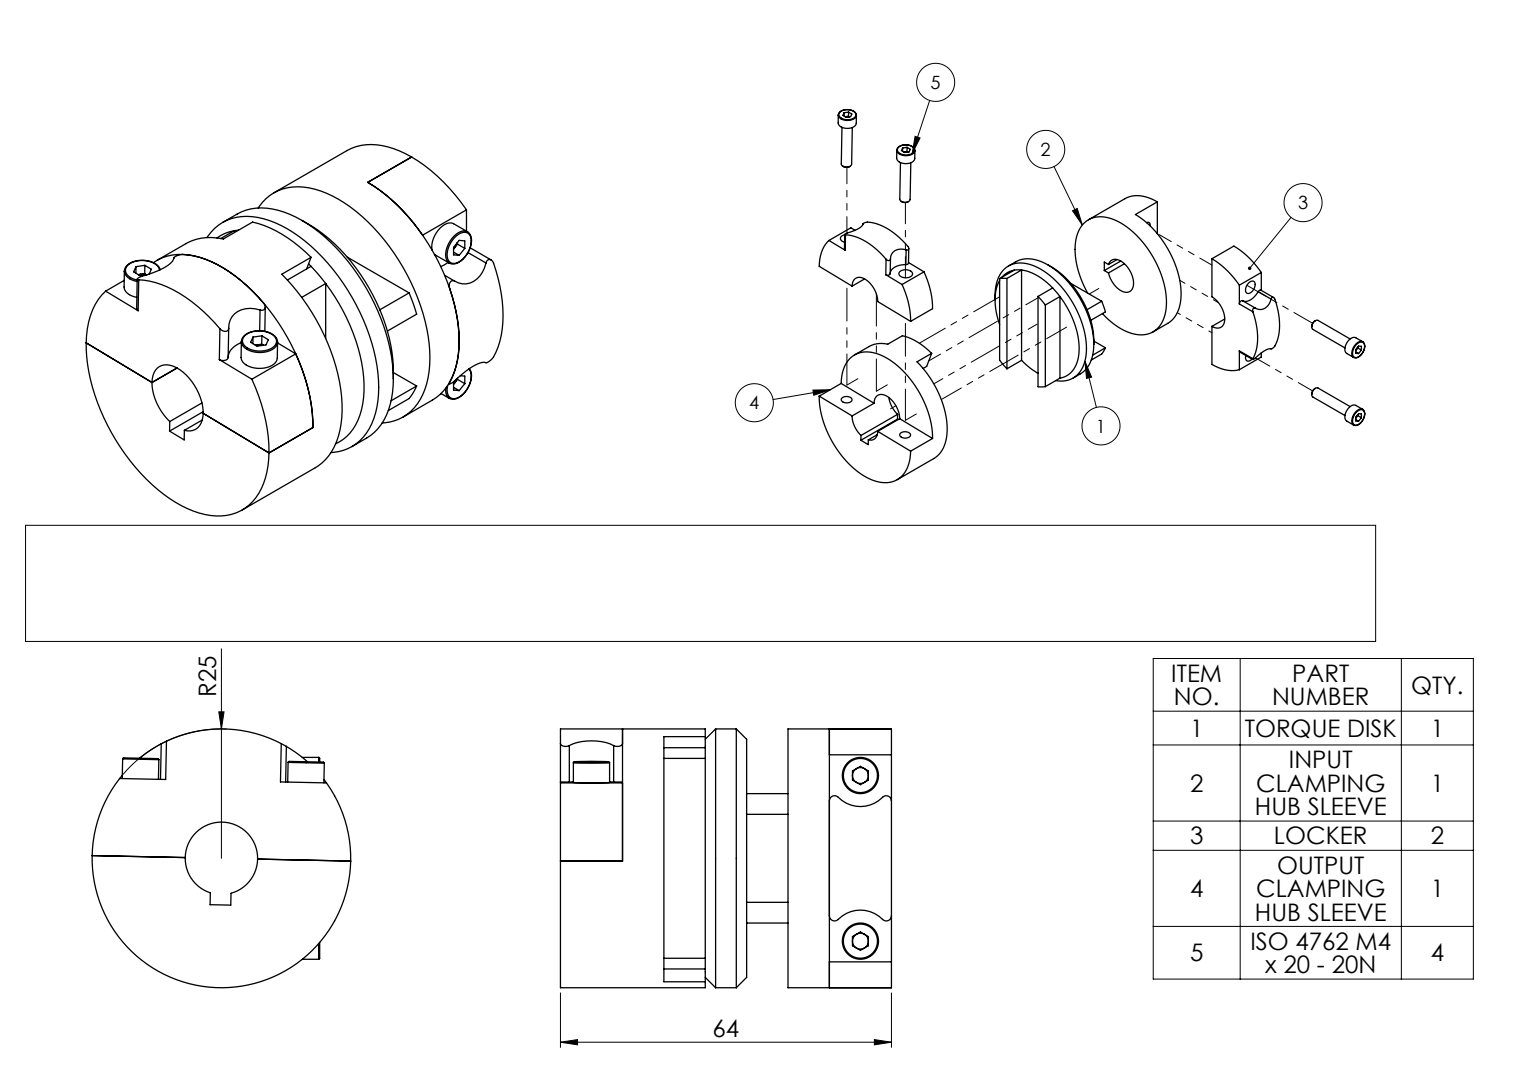
ISO-10303-21;
HEADER;
FILE_DESCRIPTION (('STEP AP214'),
    '1' );
FILE_NAME ('BR-550',
    '2026-10-08T14:09:18',
    ( '' ),
    ( '' ),
    'SwSTEP 2.0',
    'SolidWorks 2026',
    '' );
FILE_SCHEMA (( 'AUTOMOTIVE_DESIGN' ));
ENDSEC;

DATA;
#1 = LINE ( 'NONE', #1937, #4329 ) ;
#2 = CARTESIAN_POINT ( 'NONE',  ( -6.517431832507181422E-14, 16.00000000000000000, -26.00000000000000355 ) ) ;
#3 = EDGE_LOOP ( 'NONE', ( #3250, #4536, #2732 ) ) ;
#4 = CARTESIAN_POINT ( 'NONE',  ( 0.000000000000000000, 0.000000000000000000, -12.00000000000000000 ) ) ;
#5 = AXIS2_PLACEMENT_3D ( 'NONE', #3716, #3077, #4925 ) ;
#6 = AXIS2_PLACEMENT_3D ( 'NONE', #3174, #4687, #3807 ) ;
#7 = VERTEX_POINT ( 'NONE', #1885 ) ;
#8 = EDGE_CURVE ( 'NONE', #881, #1919, #4427, .T. ) ;
#9 = VERTEX_POINT ( 'NONE', #2215 ) ;
#10 =( NAMED_UNIT ( * ) PLANE_ANGLE_UNIT ( ) SI_UNIT ( $, .RADIAN. ) );
#11 = EDGE_CURVE ( 'NONE', #1059, #406, #4156, .T. ) ;
#12 = VECTOR ( 'NONE', #1631, 1000.000000000000227 ) ;
#13 = DIRECTION ( 'NONE',  ( -0.000000000000000000, -0.000000000000000000, 1.000000000000000000 ) ) ;
#14 = CIRCLE ( 'NONE', #4735, 1.535500000000000087 ) ;
#15 = CARTESIAN_POINT ( 'NONE',  ( -6.708203932499367639, 2.000000000000000888, -20.00000000000000000 ) ) ;
#16 = ORIENTED_EDGE ( 'NONE', *, *, #4419, .T. ) ;
#17 = AXIS2_PLACEMENT_3D ( 'NONE', #2780, #4294, #3843 ) ;
#18 = ADVANCED_FACE ( 'NONE', ( #4455 ), #1426, .T. ) ;
#19 = ADVANCED_FACE ( 'NONE', ( #264 ), #4482, .F. ) ;
#20 = CARTESIAN_POINT ( 'NONE',  ( 2.500000000000000000, -1.178949249685218303, -2.041999999999998039 ) ) ;
#21 = AXIS2_PLACEMENT_3D ( 'NONE', #885, #4593, #1214 ) ;
#22 = EDGE_LOOP ( 'NONE', ( #4472, #3909, #3003, #3741, #4316 ) ) ;
#23 = ORIENTED_EDGE ( 'NONE', *, *, #1515, .T. ) ;
#24 = CIRCLE ( 'NONE', #1949, 3.500000000000000000 ) ;
#25 = CARTESIAN_POINT ( 'NONE',  ( 22.89074894326665088, 10.05057747304974924, -26.80355754512474675 ) ) ;
#26 = FACE_OUTER_BOUND ( 'NONE', #3587, .T. ) ;
#27 = DIRECTION ( 'NONE',  ( 0.000000000000000000, -1.000000000000000000, 1.287488025362403787E-15 ) ) ;
#28 = CIRCLE ( 'NONE', #4350, 3.500000000000000000 ) ;
#29 = DIRECTION ( 'NONE',  ( -0.000000000000000000, -0.000000000000000000, 1.000000000000000000 ) ) ;
#30 = ORIENTED_EDGE ( 'NONE', *, *, #808, .T. ) ;
#31 = DIRECTION ( 'NONE',  ( 1.000000000000000000, 0.000000000000000000, 0.000000000000000000 ) ) ;
#32 = CARTESIAN_POINT ( 'NONE',  ( 15.00000000000000178, -16.00000000000000000, -26.00000000000000355 ) ) ;
#33 = DIRECTION ( 'NONE',  ( -0.000000000000000000, 1.000000000000000000, 1.224646799147353207E-16 ) ) ;
#34 = FACE_BOUND ( 'NONE', #887, .T. ) ;
#35 = CIRCLE ( 'NONE', #4595, 22.99999999999998934 ) ;
#36 = ORIENTED_EDGE ( 'NONE', *, *, #664, .F. ) ;
#37 = EDGE_LOOP ( 'NONE', ( #3778, #2575, #3763, #206 ) ) ;
#38 = ADVANCED_BREP_SHAPE_REPRESENTATION ( '', ( #2058, #1918 ), #1039 ) ;
#39 = DIRECTION ( 'NONE',  ( 0.000000000000000000, 0.000000000000000000, -1.000000000000000000 ) ) ;
#40 = FACE_OUTER_BOUND ( 'NONE', #1799, .T. ) ;
#41 = LINE ( 'NONE', #2781, #4907 ) ;
#42 = ORIENTED_EDGE ( 'NONE', *, *, #4705, .F. ) ;
#43 = DIRECTION ( 'NONE',  ( 1.000000000000000000, -0.000000000000000000, -0.000000000000000000 ) ) ;
#44 = LINE ( 'NONE', #3926, #164 ) ;
#45 = VERTEX_POINT ( 'NONE', #656 ) ;
#46 = PRODUCT_DEFINITION_SHAPE ( 'NONE', 'NONE',  #4967 ) ;
#47 = ADVANCED_FACE ( 'NONE', ( #2594 ), #1860, .F. ) ;
#48 = EDGE_LOOP ( 'NONE', ( #130, #2080, #1685, #2442 ) ) ;
#49 = LINE ( 'NONE', #3799, #2903 ) ;
#50 = FACE_OUTER_BOUND ( 'NONE', #3870, .T. ) ;
#51 = PRODUCT ( 'socket head cap screw_iso_ISO 4762 M5 x 20 - 20N', 'socket head cap screw_iso_ISO 4762 M5 x 20 - 20N', '', ( #972 ) ) ;
#52 = DIRECTION ( 'NONE',  ( -1.000000000000000000, -0.000000000000000000, -0.000000000000000000 ) ) ;
#53 = EDGE_CURVE ( 'NONE', #754, #3692, #3957, .T. ) ;
#54 = VERTEX_POINT ( 'NONE', #3686 ) ;
#55 = ORIENTED_EDGE ( 'NONE', *, *, #2270, .T. ) ;
#56 = DIRECTION ( 'NONE',  ( 0.000000000000000000, 0.000000000000000000, -1.000000000000000000 ) ) ;
#57 = DIRECTION ( 'NONE',  ( 1.000000000000000000, 0.000000000000000000, 0.000000000000000000 ) ) ;
#58 = FACE_OUTER_BOUND ( 'NONE', #389, .T. ) ;
#59 = ORIENTED_EDGE ( 'NONE', *, *, #2870, .T. ) ;
#60 = ORIENTED_EDGE ( 'NONE', *, *, #3152, .T. ) ;
#61 =( NAMED_UNIT ( * ) PLANE_ANGLE_UNIT ( ) SI_UNIT ( $, .RADIAN. ) );
#62 = CARTESIAN_POINT ( 'NONE',  ( 0.000000000000000000, 0.000000000000000000, 4.000000000000000000 ) ) ;
#63 = DIRECTION ( 'NONE',  ( 1.000000000000000000, -0.000000000000000000, 0.000000000000000000 ) ) ;
#64 = DIRECTION ( 'NONE',  ( 0.000000000000000000, -1.000000000000000000, 0.000000000000000000 ) ) ;
#65 = PRESENTATION_LAYER_ASSIGNMENT (  '', '', ( #1267 ) ) ;
#66 = ORIENTED_EDGE ( 'NONE', *, *, #2378, .T. ) ;
#67 = CARTESIAN_POINT ( 'NONE',  ( 25.00000000000000000, -11.80087472665741011, -21.71428571428571530 ) ) ;
#68 = EDGE_LOOP ( 'NONE', ( #4400, #3556, #1967, #1620 ) ) ;
#69 = ORIENTED_EDGE ( 'NONE', *, *, #2839, .T. ) ;
#70 = ADVANCED_FACE ( 'NONE', ( #1108 ), #102, .F. ) ;
#71 = ADVANCED_FACE ( 'NONE', ( #4306 ), #1906, .T. ) ;
#72 = CARTESIAN_POINT ( 'NONE',  ( 22.90859662698202470, -10.00982993400317334, -25.60100662543646877 ) ) ;
#73 = DIRECTION ( 'NONE',  ( 1.000000000000000000, -0.000000000000000000, -0.000000000000000000 ) ) ;
#74 = CARTESIAN_POINT ( 'NONE',  ( 2.000000000000000000, 1.329782007511006281, 0.7677499999999990443 ) ) ;
#75 = ORIENTED_EDGE ( 'NONE', *, *, #4606, .T. ) ;
#76 = AXIS2_PLACEMENT_3D ( 'NONE', #1953, #1896, #4546 ) ;
#77 = EDGE_LOOP ( 'NONE', ( #2842, #2826, #4730, #3841 ) ) ;
#78 = EDGE_CURVE ( 'NONE', #3692, #754, #3167, .T. ) ;
#79 = DIRECTION ( 'NONE',  ( 1.000000000000000000, 0.000000000000000000, 0.000000000000000000 ) ) ;
#80 = DIRECTION ( 'NONE',  ( -0.000000000000000000, -0.000000000000000000, 1.000000000000000000 ) ) ;
#81 = CARTESIAN_POINT ( 'NONE',  ( 21.90226041726126383, 12.05376714070078847, -31.32044994803182547 ) ) ;
#82 = ORIENTED_EDGE ( 'NONE', *, *, #1120, .T. ) ;
#83 = AXIS2_PLACEMENT_3D ( 'NONE', #3595, #2177, #3698 ) ;
#84 = ORIENTED_EDGE ( 'NONE', *, *, #4675, .T. ) ;
#85 = SURFACE_STYLE_FILL_AREA ( #4292 ) ;
#86 = DIRECTION ( 'NONE',  ( 1.000000000000000000, 0.000000000000000000, -0.000000000000000000 ) ) ;
#87 = DIRECTION ( 'NONE',  ( 1.357798298438996130E-15, -1.000000000000000000, 0.000000000000000000 ) ) ;
#88 = CARTESIAN_POINT ( 'NONE',  ( 15.00000000000000000, 11.10102051443364424, -21.00000000000000000 ) ) ;
#89 = AXIS2_PLACEMENT_3D ( 'NONE', #3740, #316, #1588 ) ;
#90 = ORIENTED_EDGE ( 'NONE', *, *, #4505, .T. ) ;
#91 = CIRCLE ( 'NONE', #3370, 2.099999999999997868 ) ;
#92 = VECTOR ( 'NONE', #1190, 1000.000000000000000 ) ;
#93 = LINE ( 'NONE', #2056, #2959 ) ;
#94 = DIRECTION ( 'NONE',  ( -1.000000000000000000, 0.000000000000000000, 0.000000000000000000 ) ) ;
#95 = ORIENTED_EDGE ( 'NONE', *, *, #1051, .F. ) ;
#96 = VECTOR ( 'NONE', #306, 1000.000000000000000 ) ;
#97 = VECTOR ( 'NONE', #3015, 1000.000000000000000 ) ;
#98 = ORIENTED_EDGE ( 'NONE', *, *, #3653, .F. ) ;
#99 = EDGE_CURVE ( 'NONE', #4080, #934, #4271, .T. ) ;
#100 = CIRCLE ( 'NONE', #2908, 6.999999999999999112 ) ;
#101 = AXIS2_PLACEMENT_3D ( 'NONE', #4841, #1750, #2213 ) ;
#102 = PLANE ( 'NONE',  #3242 ) ;
#103 = VECTOR ( 'NONE', #177, 1000.000000000000114 ) ;
#104 = CARTESIAN_POINT ( 'NONE',  ( 22.03949535914419755, -11.80087472665740655, -21.71428571428571885 ) ) ;
#105 = FACE_OUTER_BOUND ( 'NONE', #4278, .T. ) ;
#106 = CARTESIAN_POINT ( 'NONE',  ( 2.000000000000000000, -1.773042676681340968, 2.059984127722458425E-15 ) ) ;
#107 = VERTEX_POINT ( 'NONE', #3557 ) ;
#108 = SHAPE_DEFINITION_REPRESENTATION ( #4246, #4748 ) ;
#109 = CIRCLE ( 'NONE', #436, 17.00000000000000000 ) ;
#110 = DIRECTION ( 'NONE',  ( 0.000000000000000000, -0.4999999999999993339, 0.8660254037844389297 ) ) ;
#111 = CARTESIAN_POINT ( 'NONE',  ( -9.000000000000003553, -1.999999999999999112, -20.00000000000000000 ) ) ;
#112 = CARTESIAN_POINT ( 'NONE',  ( 0.000000000000000000, 0.000000000000000000, -20.00000000000000000 ) ) ;
#113 = EDGE_CURVE ( 'NONE', #181, #2456, #4183, .T. ) ;
#114 = ORIENTED_EDGE ( 'NONE', *, *, #457, .T. ) ;
#115 = VERTEX_POINT ( 'NONE', #877 ) ;
#116 = CARTESIAN_POINT ( 'NONE',  ( -25.00000000000000000, 3.061616997868383043E-15, -4.000000000000000000 ) ) ;
#117 = CARTESIAN_POINT ( 'NONE',  ( 0.000000000000000000, 25.00000000000000000, -20.00000000000000000 ) ) ;
#118 = AXIS2_PLACEMENT_3D ( 'NONE', #3711, #1384, #2920 ) ;
#119 = DIRECTION ( 'NONE',  ( 1.000000000000000000, 0.000000000000000000, 0.000000000000000000 ) ) ;
#120 = ADVANCED_FACE ( 'NONE', ( #2037 ), #2439, .T. ) ;
#121 = VERTEX_POINT ( 'NONE', #126 ) ;
#122 = CIRCLE ( 'NONE', #3524, 2.649999999999995914 ) ;
#123 = DIRECTION ( 'NONE',  ( -0.000000000000000000, -0.000000000000000000, -1.000000000000000000 ) ) ;
#124 = CARTESIAN_POINT ( 'NONE',  ( 16.10609822396473945, -5.439999999999995062, -4.000000000000000000 ) ) ;
#125 = EDGE_LOOP ( 'NONE', ( #685, #558, #2484, #4035, #4209, #3718, #4513, #747 ) ) ;
#126 = CARTESIAN_POINT ( 'NONE',  ( -16.10609822396473945, -5.439999999999995062, -12.00000000000000000 ) ) ;
#127 =( NAMED_UNIT ( * ) SI_UNIT ( $, .STERADIAN. ) SOLID_ANGLE_UNIT ( ) );
#128 = DIRECTION ( 'NONE',  ( 0.000000000000000000, -0.8660254037844390407, -0.4999999999999994449 ) ) ;
#129 = EDGE_LOOP ( 'NONE', ( #232, #1337, #3287, #640, #1099, #3548 ) ) ;
#130 = ORIENTED_EDGE ( 'NONE', *, *, #800, .F. ) ;
#131 = PRODUCT_DEFINITION_SHAPE ( 'NONE', 'NONE',  #4966 ) ;
#132 = DIRECTION ( 'NONE',  ( 1.000000000000000000, 2.168404344971009361E-16, 0.000000000000000000 ) ) ;
#133 = EDGE_CURVE ( 'NONE', #4849, #2456, #528, .T. ) ;
#134 = DIRECTION ( 'NONE',  ( 0.7071067811865487940, 0.000000000000000000, 0.7071067811865463515 ) ) ;
#135 = DIRECTION ( 'NONE',  ( 0.5150380749100544886, 0.000000000000000000, -0.8571673007021121116 ) ) ;
#136 = EDGE_LOOP ( 'NONE', ( #1667, #4376 ) ) ;
#137 = SHAPE_REPRESENTATION ( 'BR-550', ( #3910, #1023, #1106, #3114, #2394, #3506, #4703, #4215, #952, #1905 ), #555 ) ;
#138 = ORIENTED_EDGE ( 'NONE', *, *, #3058, .T. ) ;
#139 = SURFACE_STYLE_USAGE ( .BOTH. , #2050 ) ;
#140 = DIRECTION ( 'NONE',  ( 0.000000000000000000, 0.000000000000000000, -1.000000000000000000 ) ) ;
#141 = CYLINDRICAL_SURFACE ( 'NONE', #2344, 2.649999999999992806 ) ;
#142 = DIRECTION ( 'NONE',  ( -1.000000000000000000, 0.000000000000000000, -0.000000000000000000 ) ) ;
#143 = ORIENTED_EDGE ( 'NONE', *, *, #299, .T. ) ;
#144 = DIRECTION ( 'NONE',  ( 1.000000000000000000, -0.000000000000000000, -0.000000000000000000 ) ) ;
#145 = CARTESIAN_POINT ( 'NONE',  ( 25.00000000000000000, 11.80087472665740478, -30.28571428571428470 ) ) ;
#146 = EDGE_CURVE ( 'NONE', #3852, #4296, #1281, .T. ) ;
#147 = CARTESIAN_POINT ( 'NONE',  ( 0.000000000000000000, 0.000000000000000000, -20.00000000000000000 ) ) ;
#148 = VERTEX_POINT ( 'NONE', #905 ) ;
#149 = CARTESIAN_POINT ( 'NONE',  ( -9.999999999999975131, -16.00000000000000000, -28.10000000000000142 ) ) ;
#150 = DIRECTION ( 'NONE',  ( -1.000000000000000000, -4.073394895316987600E-15, 0.000000000000000000 ) ) ;
#151 = LINE ( 'NONE', #2483, #3855 ) ;
#152 = ORIENTED_EDGE ( 'NONE', *, *, #1724, .T. ) ;
#153 = VERTEX_POINT ( 'NONE', #3959 ) ;
#154 = FACE_OUTER_BOUND ( 'NONE', #602, .T. ) ;
#155 = CARTESIAN_POINT ( 'NONE',  ( 15.00000000000000000, 16.00000000000000000, -26.00000000000000355 ) ) ;
#156 = CARTESIAN_POINT ( 'NONE',  ( 22.03949535914419755, -11.80087472665740655, -21.71428571428571885 ) ) ;
#157 = ORIENTED_EDGE ( 'NONE', *, *, #1693, .F. ) ;
#158 = ADVANCED_FACE ( 'NONE', ( #4205 ), #2001, .F. ) ;
#159 = B_SPLINE_CURVE_WITH_KNOTS ( 'NONE', 3,
 ( #3123, #2291, #1168, #2640, #4187, #3835, #3809, #759, #1888, #81, #4617, #385, #2749, #3439, #2697, #3415 ),
 .UNSPECIFIED., .F., .F.,
 ( 4, 2, 2, 2, 2, 2, 2, 4 ),
 ( 0.000000000000000000, 0.0003092645584586380158, 0.0006185291169172760315, 0.0009277936753759139388, 0.001237058233834552063, 0.001546322792293189970, 0.001855587350751827878, 0.002474116467669114968 ),
 .UNSPECIFIED. ) ;
#160 = ORIENTED_EDGE ( 'NONE', *, *, #457, .F. ) ;
#161 = DIRECTION ( 'NONE',  ( -1.000000000000000000, 0.000000000000000000, -0.000000000000000000 ) ) ;
#162 = CARTESIAN_POINT ( 'NONE',  ( 22.40016391766193138, 11.10102051443364424, -20.00000000000000000 ) ) ;
#163 = CARTESIAN_POINT ( 'NONE',  ( 0.1999999999999987899, 0.000000000000000000, 0.000000000000000000 ) ) ;
#164 = VECTOR ( 'NONE', #508, 1000.000000000000000 ) ;
#165 = VERTEX_POINT ( 'NONE', #2693 ) ;
#166 = EDGE_CURVE ( 'NONE', #107, #941, #3578, .T. ) ;
#167 = CARTESIAN_POINT ( 'NONE',  ( -12.50000000000000178, 19.30673457630782863, 4.000000000000000000 ) ) ;
#168 = CARTESIAN_POINT ( 'NONE',  ( 23.68543856465402442, -8.000000000000003553, 14.30577747056276472 ) ) ;
#169 = AXIS2_PLACEMENT_3D ( 'NONE', #62, #3894, #4293 ) ;
#170 = ORIENTED_EDGE ( 'NONE', *, *, #708, .F. ) ;
#171 = CIRCLE ( 'NONE', #2417, 17.00000000000000000 ) ;
#172 = EDGE_CURVE ( 'NONE', #645, #1989, #1795, .T. ) ;
#173 = VECTOR ( 'NONE', #4086, 1000.000000000000000 ) ;
#174 = EDGE_CURVE ( 'NONE', #4395, #54, #1471, .T. ) ;
#175 = DIRECTION ( 'NONE',  ( 0.9474175425861609545, -0.3199999999999996181, 0.000000000000000000 ) ) ;
#176 = CIRCLE ( 'NONE', #732, 3.500000000000000000 ) ;
#177 = DIRECTION ( 'NONE',  ( -0.9474175425861605104, 0.3200000000000010059, 0.000000000000000000 ) ) ;
#178 =( GEOMETRIC_REPRESENTATION_CONTEXT ( 3 ) GLOBAL_UNCERTAINTY_ASSIGNED_CONTEXT ( ( #350 ) ) GLOBAL_UNIT_ASSIGNED_CONTEXT ( ( #3558, #3977, #127 ) ) REPRESENTATION_CONTEXT ( 'NONE', 'WORKASPACE' ) );
#179 = CARTESIAN_POINT ( 'NONE',  ( 23.00000000000000711, 2.939152317953648289E-15, 4.000000000000000000 ) ) ;
#180 = ORIENTED_EDGE ( 'NONE', *, *, #1366, .T. ) ;
#181 = VERTEX_POINT ( 'NONE', #4357 ) ;
#182 = CIRCLE ( 'NONE', #2505, 2.041999999999999815 ) ;
#183 = VECTOR ( 'NONE', #1498, 999.9999999999998863 ) ;
#184 = AXIS2_PLACEMENT_3D ( 'NONE', #4270, #4673, #3105 ) ;
#185 = CARTESIAN_POINT ( 'NONE',  ( 16.10609822396473945, -5.439999999999995062, 14.30577747056276472 ) ) ;
#186 = DIRECTION ( 'NONE',  ( 1.000000000000000000, -1.106769389831504189E-16, 0.000000000000000000 ) ) ;
#187 = AXIS2_PLACEMENT_3D ( 'NONE', #4125, #819, #1824 ) ;
#188 = CARTESIAN_POINT ( 'NONE',  ( 2.000000000000000000, 1.773042676681340968, -2.276824562219559311E-15 ) ) ;
#189 = ORIENTED_EDGE ( 'NONE', *, *, #3151, .T. ) ;
#190 = B_SPLINE_CURVE_WITH_KNOTS ( 'NONE', 3,
 ( #2928, #244, #278, #4394, #4375, #967, #201, #1739, #4801, #3276 ),
 .UNSPECIFIED., .F., .F.,
 ( 4, 2, 2, 2, 4 ),
 ( 0.000000000000000000, 0.0006190800217238748033, 0.001238160043447749607, 0.001857240065171624410, 0.002476320086895499213 ),
 .UNSPECIFIED. ) ;
#191 = VECTOR ( 'NONE', #2924, 1000.000000000000000 ) ;
#192 = ORIENTED_EDGE ( 'NONE', *, *, #1976, .T. ) ;
#193 = SURFACE_STYLE_FILL_AREA ( #525 ) ;
#194 = DIRECTION ( 'NONE',  ( 0.000000000000000000, 0.000000000000000000, -1.000000000000000000 ) ) ;
#195 = DIRECTION ( 'NONE',  ( -0.9474175425861605104, 0.3200000000000010059, 0.000000000000000000 ) ) ;
#196 = EDGE_CURVE ( 'NONE', #2273, #1203, #931, .T. ) ;
#197 = CARTESIAN_POINT ( 'NONE',  ( 24.00000000000000000, 0.000000000000000000, 0.000000000000000000 ) ) ;
#198 = ORIENTED_EDGE ( 'NONE', *, *, #2205, .T. ) ;
#199 = DIRECTION ( 'NONE',  ( -1.000000000000000000, -0.000000000000000000, -0.000000000000000000 ) ) ;
#200 = DIRECTION ( 'NONE',  ( 1.000000000000000000, 0.000000000000000000, 0.000000000000000000 ) ) ;
#201 = CARTESIAN_POINT ( 'NONE',  ( 22.04417985544613146, -11.79351823160729751, -31.74594383812769749 ) ) ;
#202 = MECHANICAL_DESIGN_GEOMETRIC_PRESENTATION_REPRESENTATION (  '', ( #2202 ), #282 ) ;
#203 = CARTESIAN_POINT ( 'NONE',  ( 2.853620410115562697E-14, 8.500000000000001776, -12.00000000000000000 ) ) ;
#204 =( NAMED_UNIT ( * ) SI_UNIT ( $, .STERADIAN. ) SOLID_ANGLE_UNIT ( ) );
#205 = CARTESIAN_POINT ( 'NONE',  ( 0.000000000000000000, 0.000000000000000000, -12.00000000000000000 ) ) ;
#206 = ORIENTED_EDGE ( 'NONE', *, *, #3845, .T. ) ;
#207 = CARTESIAN_POINT ( 'NONE',  ( -31.74999999999995737, 0.000000000000000000, 0.000000000000000000 ) ) ;
#208 = ADVANCED_FACE ( 'NONE', ( #2082 ), #4946, .F. ) ;
#209 = CARTESIAN_POINT ( 'NONE',  ( 24.00000000000000000, 0.000000000000000000, 1.610000000000000098 ) ) ;
#210 = DIRECTION ( 'NONE',  ( 0.000000000000000000, 0.000000000000000000, -1.000000000000000000 ) ) ;
#211 = ORIENTED_EDGE ( 'NONE', *, *, #1116, .F. ) ;
#212 = VERTEX_POINT ( 'NONE', #756 ) ;
#213 = CARTESIAN_POINT ( 'NONE',  ( 0.000000000000000000, -25.00000000000000000, -20.00000000000000000 ) ) ;
#214 = CARTESIAN_POINT ( 'NONE',  ( 0.2500000000000002220, 4.898587196589412829E-16, -4.000000000000000000 ) ) ;
#215 = DIRECTION ( 'NONE',  ( -0.000000000000000000, 0.000000000000000000, 1.000000000000000000 ) ) ;
#216 = VERTEX_POINT ( 'NONE', #3805 ) ;
#217 = CARTESIAN_POINT ( 'NONE',  ( -13.99999999999993250, -16.00000000000000000, -26.00000000000000355 ) ) ;
#218 = CARTESIAN_POINT ( 'NONE',  ( 4.199999999999995737, 2.449293598294707893E-16, -2.000000000000000888 ) ) ;
#219 = ORIENTED_EDGE ( 'NONE', *, *, #939, .F. ) ;
#220 = ADVANCED_FACE ( 'NONE', ( #382 ), #3087, .T. ) ;
#221 = CARTESIAN_POINT ( 'NONE',  ( 25.00000000000000000, 11.10102051443364424, -21.00000000000000000 ) ) ;
#222 = APPLICATION_PROTOCOL_DEFINITION ( 'draft international standard', 'automotive_design', 1998, #2153 ) ;
#223 = CARTESIAN_POINT ( 'NONE',  ( -7.332110811570578784E-14, -6.999999999999999112, -32.00000000000000000 ) ) ;
#224 = DIRECTION ( 'NONE',  ( -0.000000000000000000, -0.000000000000000000, 1.000000000000000000 ) ) ;
#225 = PRESENTATION_LAYER_ASSIGNMENT (  '', '', ( #3423 ) ) ;
#226 = ORIENTED_EDGE ( 'NONE', *, *, #3828, .F. ) ;
#227 = PRODUCT_RELATED_PRODUCT_CATEGORY ( 'part', '', ( #263 ) ) ;
#228 = EDGE_CURVE ( 'NONE', #497, #1504, #3710, .T. ) ;
#229 = CARTESIAN_POINT ( 'NONE',  ( 0.000000000000000000, 0.000000000000000000, -32.00000000000000000 ) ) ;
#230 = FACE_OUTER_BOUND ( 'NONE', #3929, .T. ) ;
#231 = CARTESIAN_POINT ( 'NONE',  ( 2.444036937190193033E-14, 6.999999999999999112, -20.00000000000000000 ) ) ;
#232 = ORIENTED_EDGE ( 'NONE', *, *, #1612, .F. ) ;
#233 = EDGE_CURVE ( 'NONE', #7, #497, #1330, .T. ) ;
#234 = EDGE_CURVE ( 'NONE', #1400, #1443, #448, .T. ) ;
#235 = EDGE_LOOP ( 'NONE', ( #4089, #4144 ) ) ;
#236 = VECTOR ( 'NONE', #1592, 1000.000000000000000 ) ;
#237 = DIRECTION ( 'NONE',  ( -1.000000000000000000, -0.000000000000000000, -0.000000000000000000 ) ) ;
#238 = DIRECTION ( 'NONE',  ( 1.000000000000000000, -0.000000000000000000, -0.000000000000000000 ) ) ;
#239 = DIRECTION ( 'NONE',  ( 0.000000000000000000, 0.5000000000000009992, 0.8660254037844381525 ) ) ;
#240 = VERTEX_POINT ( 'NONE', #2913 ) ;
#241 = ORIENTED_EDGE ( 'NONE', *, *, #4762, .F. ) ;
#242 = AXIS2_PLACEMENT_3D ( 'NONE', #3899, #3088, #3132 ) ;
#243 = LINE ( 'NONE', #1762, #4071 ) ;
#244 = CARTESIAN_POINT ( 'NONE',  ( 21.96482728828171460, -11.94032596560094461, -30.42234803747852467 ) ) ;
#245 = CIRCLE ( 'NONE', #405, 25.00000000000000000 ) ;
#246 = ORIENTED_EDGE ( 'NONE', *, *, #3864, .T. ) ;
#247 = CIRCLE ( 'NONE', #2817, 2.200000000000001066 ) ;
#248 = LINE ( 'NONE', #4070, #1913 ) ;
#249 = CARTESIAN_POINT ( 'NONE',  ( 2.000000000000000000, 1.773042676681340968, -2.276824562219559311E-15 ) ) ;
#250 = ITEM_DEFINED_TRANSFORMATION ( 'NONE', 'NONE', #952,  #1918 ) ;
#251 = DIRECTION ( 'NONE',  ( 1.000000000000000000, 0.000000000000000000, -0.000000000000000000 ) ) ;
#252 = DIRECTION ( 'NONE',  ( 0.000000000000000000, 0.000000000000000000, -1.000000000000000000 ) ) ;
#253 = CIRCLE ( 'NONE', #5, 2.099999999999997868 ) ;
#254 = AXIS2_PLACEMENT_3D ( 'NONE', #4822, #3198, #2921 ) ;
#255 = ORIENTED_EDGE ( 'NONE', *, *, #4921, .F. ) ;
#256 = AXIS2_PLACEMENT_3D ( 'NONE', #2633, #1779, #4840 ) ;
#257 = AXIS2_PLACEMENT_3D ( 'NONE', #3512, #3491, #493 ) ;
#258 = FACE_OUTER_BOUND ( 'NONE', #2794, .T. ) ;
#259 = DIRECTION ( 'NONE',  ( 0.000000000000000000, 0.000000000000000000, -1.000000000000000000 ) ) ;
#260 = DIRECTION ( 'NONE',  ( 1.000000000000000000, -0.000000000000000000, -0.000000000000000000 ) ) ;
#261 = AXIS2_PLACEMENT_3D ( 'NONE', #1866, #4851, #4564 ) ;
#262 = ORIENTED_EDGE ( 'NONE', *, *, #2624, .F. ) ;
#263 = PRODUCT ( 'locker', 'locker', '', ( #3647 ) ) ;
#264 = FACE_OUTER_BOUND ( 'NONE', #2383, .T. ) ;
#265 =( NAMED_UNIT ( * ) PLANE_ANGLE_UNIT ( ) SI_UNIT ( $, .RADIAN. ) );
#266 = VECTOR ( 'NONE', #64, 1000.000000000000000 ) ;
#267 = DIRECTION ( 'NONE',  ( 0.000000000000000000, -1.000000000000000000, 0.000000000000000000 ) ) ;
#268 = CIRCLE ( 'NONE', #3072, 25.00000000000000000 ) ;
#269 = LINE ( 'NONE', #4370, #3848 ) ;
#270 = FACE_OUTER_BOUND ( 'NONE', #2121, .T. ) ;
#271 = EDGE_CURVE ( 'NONE', #2827, #2641, #3245, .T. ) ;
#272 = EDGE_CURVE ( 'NONE', #4859, #4459, #35, .T. ) ;
#273 = ORIENTED_EDGE ( 'NONE', *, *, #2286, .F. ) ;
#274 = ORIENTED_EDGE ( 'NONE', *, *, #1417, .T. ) ;
#275 = MECHANICAL_DESIGN_GEOMETRIC_PRESENTATION_REPRESENTATION (  '', ( #1381 ), #2264 ) ;
#276 = DIRECTION ( 'NONE',  ( 0.000000000000000000, -0.5000000000000008882, -0.8660254037844380415 ) ) ;
#277 = CARTESIAN_POINT ( 'NONE',  ( 0.000000000000000000, 0.000000000000000000, -12.00000000000000000 ) ) ;
#278 = CARTESIAN_POINT ( 'NONE',  ( 21.90877321452243365, -12.04191644460182431, -30.60336459293191780 ) ) ;
#279 = AXIS2_PLACEMENT_3D ( 'NONE', #4796, #2900, #4321 ) ;
#280 = ORIENTED_EDGE ( 'NONE', *, *, #692, .F. ) ;
#281 = DIRECTION ( 'NONE',  ( 0.000000000000000000, 0.000000000000000000, -1.000000000000000000 ) ) ;
#282 =( GEOMETRIC_REPRESENTATION_CONTEXT ( 3 ) GLOBAL_UNCERTAINTY_ASSIGNED_CONTEXT ( ( #2248 ) ) GLOBAL_UNIT_ASSIGNED_CONTEXT ( ( #695, #1844, #4603 ) ) REPRESENTATION_CONTEXT ( 'NONE', 'WORKASPACE' ) );
#283 = ORIENTED_EDGE ( 'NONE', *, *, #1551, .T. ) ;
#284 = CARTESIAN_POINT ( 'NONE',  ( 22.76747806470418567, 10.32821797429375010, -24.00231280675427215 ) ) ;
#285 = DIRECTION ( 'NONE',  ( 0.000000000000000000, 0.4999999999999993339, -0.8660254037844390407 ) ) ;
#286 = ORIENTED_EDGE ( 'NONE', *, *, #2509, .T. ) ;
#287 = ORIENTED_EDGE ( 'NONE', *, *, #3972, .T. ) ;
#288 = EDGE_CURVE ( 'NONE', #1390, #3410, #3646, .T. ) ;
#289 = CARTESIAN_POINT ( 'NONE',  ( -9.000000000000003553, -1.999999999999999112, -32.00000000000000000 ) ) ;
#290 = PLANE ( 'NONE',  #1520 ) ;
#291 = DIRECTION ( 'NONE',  ( -1.106769389831504682E-16, -1.000000000000000000, 0.000000000000000000 ) ) ;
#292 = ORIENTED_EDGE ( 'NONE', *, *, #1706, .F. ) ;
#293 = FACE_OUTER_BOUND ( 'NONE', #4691, .T. ) ;
#294 = DIRECTION ( 'NONE',  ( 0.000000000000000000, 0.000000000000000000, -1.000000000000000000 ) ) ;
#295 = ADVANCED_FACE ( 'NONE', ( #2885 ), #673, .T. ) ;
#296 = PLANE ( 'NONE',  #570 ) ;
#297 = VERTEX_POINT ( 'NONE', #1741 ) ;
#298 = B_SPLINE_CURVE_WITH_KNOTS ( 'NONE', 3,
 ( #2171, #3292, #3229, #3661, #2073, #4458, #3590, #4061, #2542, #162 ),
 .UNSPECIFIED., .F., .F.,
 ( 4, 2, 2, 2, 4 ),
 ( 0.000000000000000000, 0.0006190800217238756707, 0.001238160043447751341, 0.001857240065171627012, 0.002476320086895502683 ),
 .UNSPECIFIED. ) ;
#299 = EDGE_CURVE ( 'NONE', #4175, #811, #2955, .T. ) ;
#300 = DIRECTION ( 'NONE',  ( 0.000000000000000000, 0.000000000000000000, -1.000000000000000000 ) ) ;
#301 = CARTESIAN_POINT ( 'NONE',  ( 0.000000000000000000, 0.000000000000000000, 12.00000000000000000 ) ) ;
#302 = CARTESIAN_POINT ( 'NONE',  ( 0.000000000000000000, 0.000000000000000000, -12.00000000000000000 ) ) ;
#303 = ORIENTED_EDGE ( 'NONE', *, *, #3258, .T. ) ;
#304 = DIRECTION ( 'NONE',  ( -1.000000000000000000, -0.000000000000000000, -0.000000000000000000 ) ) ;
#305 =( GEOMETRIC_REPRESENTATION_CONTEXT ( 3 ) GLOBAL_UNCERTAINTY_ASSIGNED_CONTEXT ( ( #1895 ) ) GLOBAL_UNIT_ASSIGNED_CONTEXT ( ( #3470, #4642, #2320 ) ) REPRESENTATION_CONTEXT ( 'NONE', 'WORKASPACE' ) );
#306 = DIRECTION ( 'NONE',  ( 1.000000000000000000, -3.578554360455197734E-15, 0.000000000000000000 ) ) ;
#307 = DIRECTION ( 'NONE',  ( 0.000000000000000000, 0.000000000000000000, -1.000000000000000000 ) ) ;
#308 = ORIENTED_EDGE ( 'NONE', *, *, #4604, .F. ) ;
#309 =( NAMED_UNIT ( * ) PLANE_ANGLE_UNIT ( ) SI_UNIT ( $, .RADIAN. ) );
#310 = DIRECTION ( 'NONE',  ( 0.000000000000000000, 1.000000000000000000, 0.000000000000000000 ) ) ;
#311 = DIRECTION ( 'NONE',  ( 0.000000000000000000, 0.000000000000000000, -1.000000000000000000 ) ) ;
#312 = CARTESIAN_POINT ( 'NONE',  ( 4.000000000000003553, 4.286263797015736595E-16, -3.500000000000000000 ) ) ;
#313 = VERTEX_POINT ( 'NONE', #4471 ) ;
#314 = CARTESIAN_POINT ( 'NONE',  ( 0.000000000000000000, 0.000000000000000000, -32.00000000000000000 ) ) ;
#315 = CARTESIAN_POINT ( 'NONE',  ( 5.000000000000004441, 0.000000000000000000, 4.250000000000000000 ) ) ;
#316 = DIRECTION ( 'NONE',  ( -1.000000000000000000, -0.000000000000000000, -0.000000000000000000 ) ) ;
#317 = VECTOR ( 'NONE', #4957, 1000.000000000000000 ) ;
#318 = VERTEX_POINT ( 'NONE', #4781 ) ;
#319 = PLANE ( 'NONE',  #4799 ) ;
#320 = PLANE ( 'NONE',  #4355 ) ;
#321 = PLANE ( 'NONE',  #826 ) ;
#322 = EDGE_CURVE ( 'NONE', #2990, #2143, #2362, .T. ) ;
#323 = EDGE_CURVE ( 'NONE', #1722, #1339, #2532, .T. ) ;
#324 = EDGE_LOOP ( 'NONE', ( #3270, #945 ) ) ;
#325 = TOROIDAL_SURFACE ( 'NONE', #3441, 2.200000000000001066, 0.2000000000000000111 ) ;
#326 = CARTESIAN_POINT ( 'NONE',  ( 0.000000000000000000, 25.00000000000000000, -20.00000000000000000 ) ) ;
#327 = CIRCLE ( 'NONE', #3446, 2.099999999999990763 ) ;
#328 = DIRECTION ( 'NONE',  ( -0.000000000000000000, -0.000000000000000000, 1.000000000000000000 ) ) ;
#329 = LINE ( 'NONE', #4502, #575 ) ;
#330 = CARTESIAN_POINT ( 'NONE',  ( -31.74999999999995737, 0.000000000000000000, 0.000000000000000000 ) ) ;
#331 = EDGE_LOOP ( 'NONE', ( #1142, #2436, #2467, #3469, #3020 ) ) ;
#332 = VECTOR ( 'NONE', #3365, 999.9999999999998863 ) ;
#333 = DIRECTION ( 'NONE',  ( 0.000000000000000000, 0.000000000000000000, 1.000000000000000000 ) ) ;
#334 = DIRECTION ( 'NONE',  ( 9.765537692533071851E-17, -9.974667427877440261E-17, 1.000000000000000000 ) ) ;
#335 = CYLINDRICAL_SURFACE ( 'NONE', #4166, 25.00000000000000000 ) ;
#336 = CARTESIAN_POINT ( 'NONE',  ( -7.332110811570578784E-14, -6.999999999999999112, -32.00000000000000000 ) ) ;
#337 = VECTOR ( 'NONE', #2303, 999.9999999999998863 ) ;
#338 = DIRECTION ( 'NONE',  ( 0.000000000000000000, 0.000000000000000000, -1.000000000000000000 ) ) ;
#339 = AXIS2_PLACEMENT_3D ( 'NONE', #3312, #4913, #3750 ) ;
#340 = VERTEX_POINT ( 'NONE', #1371 ) ;
#341 = CIRCLE ( 'NONE', #1452, 2.700000000000001066 ) ;
#342 = VECTOR ( 'NONE', #2797, 1000.000000000000000 ) ;
#343 = MECHANICAL_DESIGN_GEOMETRIC_PRESENTATION_REPRESENTATION (  '', ( #3776 ), #4337 ) ;
#344 = FACE_OUTER_BOUND ( 'NONE', #964, .T. ) ;
#345 = ADVANCED_BREP_SHAPE_REPRESENTATION ( '', ( #3609, #1918 ), #305 ) ;
#346 = DIRECTION ( 'NONE',  ( -1.000000000000000000, -0.000000000000000000, -0.000000000000000000 ) ) ;
#347 =( NAMED_UNIT ( * ) PLANE_ANGLE_UNIT ( ) SI_UNIT ( $, .RADIAN. ) );
#348 = CIRCLE ( 'NONE', #3779, 4.000000000000000000 ) ;
#349 = ORIENTED_EDGE ( 'NONE', *, *, #1643, .T. ) ;
#350 = UNCERTAINTY_MEASURE_WITH_UNIT (LENGTH_MEASURE( 1.000000000000000082E-05 ), #3558, 'distance_accuracy_value', 'NONE');
#351 = DIRECTION ( 'NONE',  ( 0.9474175425861605104, 0.3200000000000010059, 0.000000000000000000 ) ) ;
#352 = ADVANCED_FACE ( 'NONE', ( #4835 ), #4072, .F. ) ;
#353 = SURFACE_STYLE_FILL_AREA ( #4217 ) ;
#354 = CONTEXT_DEPENDENT_SHAPE_REPRESENTATION ( #3840, #3755 ) ;
#355 = ADVANCED_FACE ( 'NONE', ( #643 ), #4445, .F. ) ;
#356 = EDGE_LOOP ( 'NONE', ( #4695, #2450 ) ) ;
#357 = DIRECTION ( 'NONE',  ( 0.9474175425861609545, 0.3199999999999996181, -0.000000000000000000 ) ) ;
#358 = PLANE ( 'NONE',  #2103 ) ;
#359 = DIRECTION ( 'NONE',  ( -0.000000000000000000, -0.000000000000000000, 1.000000000000000000 ) ) ;
#360 = ORIENTED_EDGE ( 'NONE', *, *, #3573, .F. ) ;
#361 = AXIS2_PLACEMENT_3D ( 'NONE', #2287, #1500, #3043 ) ;
#362 = EDGE_CURVE ( 'NONE', #1707, #1968, #2444, .T. ) ;
#363 = EDGE_LOOP ( 'NONE', ( #280, #2338, #1740, #3798 ) ) ;
#364 = DIRECTION ( 'NONE',  ( 0.000000000000000000, 0.000000000000000000, -1.000000000000000000 ) ) ;
#365 = FACE_OUTER_BOUND ( 'NONE', #770, .T. ) ;
#366 = CARTESIAN_POINT ( 'NONE',  ( 0.000000000000000000, 0.000000000000000000, 3.299999999999999822 ) ) ;
#367 = ORIENTED_EDGE ( 'NONE', *, *, #4173, .F. ) ;
#368 = DIRECTION ( 'NONE',  ( -1.000000000000000000, -0.000000000000000000, -0.000000000000000000 ) ) ;
#369 = CARTESIAN_POINT ( 'NONE',  ( -9.999999999999975131, -16.00000000000000000, -28.10000000000000142 ) ) ;
#370 = CARTESIAN_POINT ( 'NONE',  ( 0.000000000000000000, 0.000000000000000000, -32.00000000000000000 ) ) ;
#371 = ORIENTED_EDGE ( 'NONE', *, *, #1787, .F. ) ;
#372 = DIRECTION ( 'NONE',  ( 0.000000000000000000, 0.000000000000000000, 1.000000000000000000 ) ) ;
#373 = LINE ( 'NONE', #1177, #566 ) ;
#374 = VERTEX_POINT ( 'NONE', #1802 ) ;
#375 = CARTESIAN_POINT ( 'NONE',  ( 22.61674500023159240, -10.65336738338371347, -28.73004557699725936 ) ) ;
#376 = PLANE ( 'NONE',  #1226 ) ;
#377 = CARTESIAN_POINT ( 'NONE',  ( -6.708203932499367639, 2.000000000000000888, -12.00000000000000000 ) ) ;
#378 = DIRECTION ( 'NONE',  ( 1.000000000000000000, -0.000000000000000000, -0.000000000000000000 ) ) ;
#379 = EDGE_CURVE ( 'NONE', #803, #3915, #997, .T. ) ;
#380 = ORIENTED_EDGE ( 'NONE', *, *, #2599, .F. ) ;
#381 = ADVANCED_FACE ( 'NONE', ( #1705 ), #3239, .T. ) ;
#382 = FACE_OUTER_BOUND ( 'NONE', #4619, .T. ) ;
#383 = CARTESIAN_POINT ( 'NONE',  ( 24.00000000000000000, 0.000000000000000000, 0.000000000000000000 ) ) ;
#384 = DIRECTION ( 'NONE',  ( 1.000000000000000000, -3.578554360455197734E-15, 0.000000000000000000 ) ) ;
#385 = CARTESIAN_POINT ( 'NONE',  ( 21.87320774003120150, 12.10631999347636167, -31.01543084472370992 ) ) ;
#386 = ADVANCED_FACE ( 'NONE', ( #971 ), #1098, .T. ) ;
#387 = ADVANCED_FACE ( 'NONE', ( #2250 ), #4495, .F. ) ;
#388 = ORIENTED_EDGE ( 'NONE', *, *, #3153, .T. ) ;
#389 = EDGE_LOOP ( 'NONE', ( #2947, #665, #449, #3173, #4854, #2496, #2657, #940, #4548 ) ) ;
#390 = LINE ( 'NONE', #1915, #2331 ) ;
#391 = DIRECTION ( 'NONE',  ( 0.000000000000000000, 0.000000000000000000, 1.000000000000000000 ) ) ;
#392 = VERTEX_POINT ( 'NONE', #3773 ) ;
#393 = UNCERTAINTY_MEASURE_WITH_UNIT (LENGTH_MEASURE( 1.000000000000000082E-05 ), #500, 'distance_accuracy_value', 'NONE');
#394 = CARTESIAN_POINT ( 'NONE',  ( 15.00000000000000000, 11.10102051443364424, -20.00000000000000000 ) ) ;
#395 = CARTESIAN_POINT ( 'NONE',  ( -3.642919299551294898E-14, -16.00000000000000000, -26.00000000000000355 ) ) ;
#396 = CIRCLE ( 'NONE', #2236, 25.00000000000000000 ) ;
#397 = ORIENTED_EDGE ( 'NONE', *, *, #3827, .F. ) ;
#398 = VERTEX_POINT ( 'NONE', #2707 ) ;
#399 = CIRCLE ( 'NONE', #3208, 2.099999999999997868 ) ;
#400 = EDGE_CURVE ( 'NONE', #2569, #4849, #4958, .T. ) ;
#401 = DIRECTION ( 'NONE',  ( -1.000000000000000000, -0.000000000000000000, -0.000000000000000000 ) ) ;
#402 = DIRECTION ( 'NONE',  ( 1.000000000000000000, 2.036697447658493800E-15, 0.000000000000000000 ) ) ;
#403 = CYLINDRICAL_SURFACE ( 'NONE', #418, 23.00000000000000711 ) ;
#404 = LINE ( 'NONE', #3458, #2987 ) ;
#405 = AXIS2_PLACEMENT_3D ( 'NONE', #4519, #1873, #1469 ) ;
#406 = VERTEX_POINT ( 'NONE', #2208 ) ;
#407 = VECTOR ( 'NONE', #816, 1000.000000000000000 ) ;
#408 = DIRECTION ( 'NONE',  ( 0.000000000000000000, 0.5000000000000011102, 0.8660254037844380415 ) ) ;
#409 = DIRECTION ( 'NONE',  ( 1.000000000000000000, 0.000000000000000000, 0.000000000000000000 ) ) ;
#410 = DIRECTION ( 'NONE',  ( 0.000000000000000000, 0.000000000000000000, -1.000000000000000000 ) ) ;
#411 = CARTESIAN_POINT ( 'NONE',  ( 0.000000000000000000, 0.000000000000000000, -20.00000000000000000 ) ) ;
#412 = CARTESIAN_POINT ( 'NONE',  ( 0.000000000000000000, 0.000000000000000000, -1.999999999999994893 ) ) ;
#413 = AXIS2_PLACEMENT_3D ( 'NONE', #411, #1607, #4207 ) ;
#414 = CONICAL_SURFACE ( 'NONE', #1848, 2.099999999999997868, 1.029744258676653423 ) ;
#415 = ORIENTED_EDGE ( 'NONE', *, *, #196, .T. ) ;
#416 = ORIENTED_EDGE ( 'NONE', *, *, #3654, .T. ) ;
#417 = FILL_AREA_STYLE ('',( #3127 ) ) ;
#418 = AXIS2_PLACEMENT_3D ( 'NONE', #1930, #2739, #4659 ) ;
#419 = DIRECTION ( 'NONE',  ( -0.000000000000000000, -0.000000000000000000, -1.000000000000000000 ) ) ;
#420 = MECHANICAL_DESIGN_GEOMETRIC_PRESENTATION_REPRESENTATION (  '', ( #1141 ), #178 ) ;
#421 = ADVANCED_FACE ( 'NONE', ( #3011 ), #320, .F. ) ;
#422 = DIRECTION ( 'NONE',  ( -0.000000000000000000, -0.000000000000000000, 1.000000000000000000 ) ) ;
#423 = CARTESIAN_POINT ( 'NONE',  ( 6.999999999999999112, 0.000000000000000000, -20.00000000000000000 ) ) ;
#424 = ORIENTED_EDGE ( 'NONE', *, *, #3827, .T. ) ;
#425 = MANIFOLD_SOLID_BREP ( 'M5 Tapped Hole1', #4581 ) ;
#426 = VECTOR ( 'NONE', #276, 1000.000000000000227 ) ;
#427 = CIRCLE ( 'NONE', #3306, 2.649999999999985700 ) ;
#428 = MECHANICAL_DESIGN_GEOMETRIC_PRESENTATION_REPRESENTATION (  '', ( #3228 ), #980 ) ;
#429 = CARTESIAN_POINT ( 'NONE',  ( 0.000000000000000000, 0.000000000000000000, -32.00000000000000000 ) ) ;
#430 = EDGE_CURVE ( 'NONE', #3154, #4346, #3398, .T. ) ;
#431 = DIRECTION ( 'NONE',  ( 0.000000000000000000, 0.000000000000000000, -1.000000000000000000 ) ) ;
#432 = AXIS2_PLACEMENT_3D ( 'NONE', #1311, #2846, #832 ) ;
#433 = AXIS2_PLACEMENT_3D ( 'NONE', #3834, #2370, #2015 ) ;
#434 = ORIENTED_EDGE ( 'NONE', *, *, #1360, .F. ) ;
#435 = ORIENTED_EDGE ( 'NONE', *, *, #3052, .T. ) ;
#436 = AXIS2_PLACEMENT_3D ( 'NONE', #2401, #1271, #4371 ) ;
#437 = CARTESIAN_POINT ( 'NONE',  ( 22.66008913276283820, 10.56067522606771547, -28.54043899563736986 ) ) ;
#438 = PLANE ( 'NONE',  #1771 ) ;
#439 = DIRECTION ( 'NONE',  ( -0.000000000000000000, -0.000000000000000000, 1.000000000000000000 ) ) ;
#440 = DIRECTION ( 'NONE',  ( 0.000000000000000000, 0.000000000000000000, 1.000000000000000000 ) ) ;
#441 = EDGE_LOOP ( 'NONE', ( #4562, #4641 ) ) ;
#442 = EDGE_LOOP ( 'NONE', ( #1911, #3869, #3953, #75 ) ) ;
#443 =( LENGTH_UNIT ( ) NAMED_UNIT ( * ) SI_UNIT ( .MILLI., .METRE. ) );
#444 = DIRECTION ( 'NONE',  ( -0.000000000000000000, -0.000000000000000000, -1.000000000000000000 ) ) ;
#445 = CARTESIAN_POINT ( 'NONE',  ( 0.000000000000000000, 0.000000000000000000, -12.00000000000000000 ) ) ;
#446 = DIRECTION ( 'NONE',  ( 0.000000000000000000, -0.5000000000000008882, -0.8660254037844380415 ) ) ;
#447 = DIRECTION ( 'NONE',  ( -1.000000000000000000, -0.000000000000000000, -0.000000000000000000 ) ) ;
#448 = CIRCLE ( 'NONE', #1077, 22.99999999999998934 ) ;
#449 = ORIENTED_EDGE ( 'NONE', *, *, #2315, .T. ) ;
#450 = EDGE_CURVE ( 'NONE', #1059, #4052, #4677, .T. ) ;
#451 = VERTEX_POINT ( 'NONE', #717 ) ;
#452 = PRESENTATION_STYLE_ASSIGNMENT (( #3871 ) ) ;
#453 = CARTESIAN_POINT ( 'NONE',  ( 0.000000000000000000, 0.000000000000000000, 4.000000000000000000 ) ) ;
#454 = DIRECTION ( 'NONE',  ( -0.000000000000000000, 0.000000000000000000, 1.000000000000000000 ) ) ;
#455 = DIRECTION ( 'NONE',  ( 0.000000000000000000, -1.000000000000000000, 1.287488025362403787E-15 ) ) ;
#456 = ORIENTED_EDGE ( 'NONE', *, *, #4832, .F. ) ;
#457 = EDGE_CURVE ( 'NONE', #181, #2569, #122, .T. ) ;
#458 = LINE ( 'NONE', #766, #3279 ) ;
#459 = DIRECTION ( 'NONE',  ( 1.000000000000000000, -0.000000000000000000, -0.000000000000000000 ) ) ;
#460 = ORIENTED_EDGE ( 'NONE', *, *, #523, .T. ) ;
#461 = ORIENTED_EDGE ( 'NONE', *, *, #692, .T. ) ;
#462 = EDGE_CURVE ( 'NONE', #3903, #3640, #245, .T. ) ;
#463 = EDGE_CURVE ( 'NONE', #519, #313, #373, .T. ) ;
#464 = CARTESIAN_POINT ( 'NONE',  ( 22.88998946896871445, 10.05230818559221539, -25.18361442742383360 ) ) ;
#465 = FILL_AREA_STYLE_COLOUR ( '', #4492 ) ;
#466 = CARTESIAN_POINT ( 'NONE',  ( 0.000000000000000000, 1.178949249685213863, -2.042000000000001148 ) ) ;
#467 = VERTEX_POINT ( 'NONE', #1823 ) ;
#468 = VERTEX_POINT ( 'NONE', #3797 ) ;
#469 = ADVANCED_BREP_SHAPE_REPRESENTATION ( '', ( #425, #1918 ), #4450 ) ;
#470 = CARTESIAN_POINT ( 'NONE',  ( 12.50000000000000178, 19.30673457630782863, 12.00000000000000000 ) ) ;
#471 = FACE_OUTER_BOUND ( 'NONE', #854, .T. ) ;
#472 = CARTESIAN_POINT ( 'NONE',  ( 21.87533763385574659, -12.10248395817102107, -21.08882388928228835 ) ) ;
#473 = ORIENTED_EDGE ( 'NONE', *, *, #4769, .F. ) ;
#474 =( NAMED_UNIT ( * ) SI_UNIT ( $, .STERADIAN. ) SOLID_ANGLE_UNIT ( ) );
#475 = DIRECTION ( 'NONE',  ( 0.000000000000000000, 0.000000000000000000, 1.000000000000000000 ) ) ;
#476 = DIRECTION ( 'NONE',  ( 0.000000000000000000, 0.000000000000000000, -1.000000000000000000 ) ) ;
#477 = LINE ( 'NONE', #4645, #4099 ) ;
#478 = STYLED_ITEM ( 'NONE', ( #1032 ), #996 ) ;
#479 = VERTEX_POINT ( 'NONE', #1438 ) ;
#480 = DIRECTION ( 'NONE',  ( 0.000000000000000000, 0.000000000000000000, 1.000000000000000000 ) ) ;
#481 = DIRECTION ( 'NONE',  ( 0.000000000000000000, -0.5000000000000012212, -0.8660254037844380415 ) ) ;
#482 = EDGE_LOOP ( 'NONE', ( #3289, #3577, #3645, #3311 ) ) ;
#483 = ADVANCED_FACE ( 'NONE', ( #2985 ), #1043, .F. ) ;
#484 = VERTEX_POINT ( 'NONE', #4908 ) ;
#485 = PRODUCT_DEFINITION_CONTEXT ( 'detailed design', #2667, 'design' ) ;
#486 = CARTESIAN_POINT ( 'NONE',  ( 22.31344532614783205, -11.27701289969359522, -22.27898711539451071 ) ) ;
#487 = EDGE_CURVE ( 'NONE', #468, #1707, #3426, .T. ) ;
#488 = LINE ( 'NONE', #3935, #3383 ) ;
#489 = EDGE_CURVE ( 'NONE', #3217, #2692, #1229, .T. ) ;
#490 = LINE ( 'NONE', #2006, #2180 ) ;
#491 = ORIENTED_EDGE ( 'NONE', *, *, #4912, .F. ) ;
#492 = SHAPE_DEFINITION_REPRESENTATION ( #1211, #4221 ) ;
#493 = DIRECTION ( 'NONE',  ( 1.000000000000000000, 0.000000000000000000, -0.000000000000000000 ) ) ;
#494 = ADVANCED_FACE ( 'NONE', ( #851 ), #1302, .F. ) ;
#495 = LINE ( 'NONE', #1938, #2572 ) ;
#496 = CYLINDRICAL_SURFACE ( 'NONE', #2581, 6.999999999999999112 ) ;
#497 = VERTEX_POINT ( 'NONE', #4679 ) ;
#498 = AXIS2_PLACEMENT_3D ( 'NONE', #873, #431, #3187 ) ;
#499 = ORIENTED_EDGE ( 'NONE', *, *, #2997, .T. ) ;
#500 =( LENGTH_UNIT ( ) NAMED_UNIT ( * ) SI_UNIT ( .MILLI., .METRE. ) );
#501 = CARTESIAN_POINT ( 'NONE',  ( -12.49999999999999822, -19.30673457630782863, 12.00000000000000000 ) ) ;
#502 = DIRECTION ( 'NONE',  ( -0.000000000000000000, -0.000000000000000000, 1.000000000000000000 ) ) ;
#503 = AXIS2_PLACEMENT_3D ( 'NONE', #890, #2321, #39 ) ;
#504 = EDGE_LOOP ( 'NONE', ( #3356, #2233, #3231, #687, #2325, #2539 ) ) ;
#505 = AXIS2_PLACEMENT_3D ( 'NONE', #2463, #2918, #1335 ) ;
#506 = VECTOR ( 'NONE', #1907, 1000.000000000000000 ) ;
#507 = DIRECTION ( 'NONE',  ( -1.000000000000000000, 0.000000000000000000, 0.000000000000000000 ) ) ;
#508 = DIRECTION ( 'NONE',  ( -1.000000000000000000, -0.000000000000000000, -0.000000000000000000 ) ) ;
#509 = ORIENTED_EDGE ( 'NONE', *, *, #4882, .F. ) ;
#510 = VECTOR ( 'NONE', #740, 1000.000000000000000 ) ;
#511 = CIRCLE ( 'NONE', #1053, 6.999999999999999112 ) ;
#512 = ORIENTED_EDGE ( 'NONE', *, *, #1917, .T. ) ;
#513 = EDGE_CURVE ( 'NONE', #4266, #3976, #2404, .T. ) ;
#514 = CARTESIAN_POINT ( 'NONE',  ( 8.500000000000003553, 21.37171027316251681, 12.00000000000000000 ) ) ;
#515 = CARTESIAN_POINT ( 'NONE',  ( 25.00000000000000000, 0.000000000000000000, 0.000000000000000000 ) ) ;
#516 = DIRECTION ( 'NONE',  ( 1.000000000000000000, -0.000000000000000000, -0.000000000000000000 ) ) ;
#517 = ORIENTED_EDGE ( 'NONE', *, *, #3654, .F. ) ;
#518 = CIRCLE ( 'NONE', #1149, 17.00000000000000000 ) ;
#519 = VERTEX_POINT ( 'NONE', #3555 ) ;
#520 = DIRECTION ( 'NONE',  ( 0.000000000000000000, 0.000000000000000000, -1.000000000000000000 ) ) ;
#521 = CARTESIAN_POINT ( 'NONE',  ( 2.500000000000000000, -1.178949249685213863, 2.042000000000002924 ) ) ;
#522 = DIRECTION ( 'NONE',  ( 1.000000000000000000, -0.000000000000000000, -0.000000000000000000 ) ) ;
#523 = EDGE_CURVE ( 'NONE', #852, #654, #2199, .T. ) ;
#524 = ORIENTED_EDGE ( 'NONE', *, *, #2305, .F. ) ;
#525 = FILL_AREA_STYLE ('',( #2096 ) ) ;
#526 = LINE ( 'NONE', #3569, #722 ) ;
#527 = CARTESIAN_POINT ( 'NONE',  ( 0.000000000000000000, -1.999999999999999112, -12.00000000000000000 ) ) ;
#528 = CIRCLE ( 'NONE', #4589, 2.649999999999985700 ) ;
#529 = FACE_OUTER_BOUND ( 'NONE', #1640, .T. ) ;
#530 = ORIENTED_EDGE ( 'NONE', *, *, #1162, .F. ) ;
#531 = CARTESIAN_POINT ( 'NONE',  ( -7.332110811570578784E-14, -6.999999999999999112, -20.00000000000000000 ) ) ;
#532 = CARTESIAN_POINT ( 'NONE',  ( -9.999999999999975131, -16.00000000000000000, -26.00000000000000355 ) ) ;
#533 = ORIENTED_EDGE ( 'NONE', *, *, #715, .T. ) ;
#534 = DIRECTION ( 'NONE',  ( -1.000000000000000000, -0.000000000000000000, -0.000000000000000000 ) ) ;
#535 = EDGE_CURVE ( 'NONE', #1202, #406, #2812, .T. ) ;
#536 = VERTEX_POINT ( 'NONE', #1955 ) ;
#537 = VERTEX_POINT ( 'NONE', #3576 ) ;
#538 = DIRECTION ( 'NONE',  ( 0.000000000000000000, 0.000000000000000000, -1.000000000000000000 ) ) ;
#539 = CARTESIAN_POINT ( 'NONE',  ( 3.999999999999997335, 2.694222958124178486E-16, 2.200000000000001066 ) ) ;
#540 = DIRECTION ( 'NONE',  ( 1.000000000000000000, 0.000000000000000000, 0.000000000000000000 ) ) ;
#541 = EDGE_CURVE ( 'NONE', #4479, #4279, #1671, .T. ) ;
#542 = ORIENTED_EDGE ( 'NONE', *, *, #78, .F. ) ;
#543 = ORIENTED_EDGE ( 'NONE', *, *, #2810, .F. ) ;
#544 =( NAMED_UNIT ( * ) PLANE_ANGLE_UNIT ( ) SI_UNIT ( $, .RADIAN. ) );
#545 = PLANE ( 'NONE',  #2901 ) ;
#546 = DIRECTION ( 'NONE',  ( -0.000000000000000000, -0.000000000000000000, 1.000000000000000000 ) ) ;
#547 = EDGE_CURVE ( 'NONE', #2929, #3315, #44, .T. ) ;
#548 = EDGE_CURVE ( 'NONE', #3988, #553, #2328, .T. ) ;
#549 = ORIENTED_EDGE ( 'NONE', *, *, #463, .T. ) ;
#550 = FACE_OUTER_BOUND ( 'NONE', #3936, .T. ) ;
#551 = CARTESIAN_POINT ( 'NONE',  ( -7.332110811570578784E-14, -6.999999999999999112, -32.00000000000000000 ) ) ;
#552 = PRESENTATION_LAYER_ASSIGNMENT (  '', '', ( #4381 ) ) ;
#553 = VERTEX_POINT ( 'NONE', #4700 ) ;
#554 = DIRECTION ( 'NONE',  ( -0.9474175425861605104, -0.3200000000000010059, 0.000000000000000000 ) ) ;
#555 =( GEOMETRIC_REPRESENTATION_CONTEXT ( 3 ) GLOBAL_UNCERTAINTY_ASSIGNED_CONTEXT ( ( #1328 ) ) GLOBAL_UNIT_ASSIGNED_CONTEXT ( ( #443, #2391, #2135 ) ) REPRESENTATION_CONTEXT ( 'NONE', 'WORKASPACE' ) );
#556 = DIRECTION ( 'NONE',  ( 1.000000000000000000, 0.000000000000000000, 0.000000000000000000 ) ) ;
#557 = ORIENTED_EDGE ( 'NONE', *, *, #3777, .T. ) ;
#558 = ORIENTED_EDGE ( 'NONE', *, *, #1089, .T. ) ;
#559 = CARTESIAN_POINT ( 'NONE',  ( 0.000000000000000000, 25.00000000000000000, -32.00000000000000000 ) ) ;
#560 = FACE_BOUND ( 'NONE', #4671, .T. ) ;
#561 = DIRECTION ( 'NONE',  ( 1.000000000000000000, -1.892318758829013864E-15, 0.000000000000000000 ) ) ;
#562 = ORIENTED_EDGE ( 'NONE', *, *, #3354, .F. ) ;
#563 = ORIENTED_EDGE ( 'NONE', *, *, #3713, .T. ) ;
#564 = CARTESIAN_POINT ( 'NONE',  ( 2.500000000000000000, 2.357898499370433054, -1.951563910473907981E-15 ) ) ;
#565 = CARTESIAN_POINT ( 'NONE',  ( 23.68543856465402442, -8.000000000000003553, -4.000000000000000000 ) ) ;
#566 = VECTOR ( 'NONE', #4170, 1000.000000000000114 ) ;
#567 = ORIENTED_EDGE ( 'NONE', *, *, #4261, .F. ) ;
#568 = CARTESIAN_POINT ( 'NONE',  ( 0.000000000000000000, 0.000000000000000000, -4.000000000000000000 ) ) ;
#569 = FACE_OUTER_BOUND ( 'NONE', #2980, .T. ) ;
#570 = AXIS2_PLACEMENT_3D ( 'NONE', #1893, #4491, #1117 ) ;
#571 = VERTEX_POINT ( 'NONE', #1569 ) ;
#572 = AXIS2_PLACEMENT_3D ( 'NONE', #2796, #33, #1986 ) ;
#573 = CARTESIAN_POINT ( 'NONE',  ( -17.00000000000000000, 0.000000000000000000, 14.30577747056276472 ) ) ;
#574 = PRODUCT_CONTEXT ( 'NONE', #3334, 'mechanical' ) ;
#575 = VECTOR ( 'NONE', #2937, 1000.000000000000000 ) ;
#576 = VECTOR ( 'NONE', #357, 1000.000000000000114 ) ;
#577 = ORIENTED_EDGE ( 'NONE', *, *, #1279, .T. ) ;
#578 = VECTOR ( 'NONE', #4525, 1000.000000000000000 ) ;
#579 = AXIS2_PLACEMENT_3D ( 'NONE', #2046, #3223, #4745 ) ;
#580 = COLOUR_RGB ( '', 0.72549020, 0.75294118, 0.79215686) ;
#581 = DIRECTION ( 'NONE',  ( 1.000000000000000000, -3.578554360455197734E-15, 0.000000000000000000 ) ) ;
#582 = CYLINDRICAL_SURFACE ( 'NONE', #2017, 25.00000000000000000 ) ;
#583 = AXIS2_PLACEMENT_3D ( 'NONE', #4630, #73, #1654 ) ;
#584 = EDGE_LOOP ( 'NONE', ( #3424, #607, #226, #4068, #1963 ) ) ;
#585 = CIRCLE ( 'NONE', #1233, 22.99999999999998934 ) ;
#586 = VERTEX_POINT ( 'NONE', #1997 ) ;
#587 = DIRECTION ( 'NONE',  ( 0.000000000000000000, 0.000000000000000000, 1.000000000000000000 ) ) ;
#588 = DIRECTION ( 'NONE',  ( 0.000000000000000000, 0.000000000000000000, 1.000000000000000000 ) ) ;
#589 = ORIENTED_EDGE ( 'NONE', *, *, #3682, .F. ) ;
#590 = CARTESIAN_POINT ( 'NONE',  ( 2.853620410115562697E-14, 8.500000000000001776, -4.000000000000000000 ) ) ;
#591 = ORIENTED_EDGE ( 'NONE', *, *, #4411, .T. ) ;
#592 = DIRECTION ( 'NONE',  ( -1.000000000000000000, -0.000000000000000000, -0.000000000000000000 ) ) ;
#593 = CARTESIAN_POINT ( 'NONE',  ( -9.000000000000001776, 2.000000000000000000, -20.00000000000000000 ) ) ;
#594 = AXIS2_PLACEMENT_3D ( 'NONE', #1405, #1084, #1809 ) ;
#595 = CARTESIAN_POINT ( 'NONE',  ( 2.000000000000000000, 0.000000000000000000, 0.000000000000000000 ) ) ;
#596 = PRODUCT_DEFINITION ( 'UNKNOWN', '', #1030, #4629 ) ;
#597 = VERTEX_POINT ( 'NONE', #124 ) ;
#598 = ADVANCED_FACE ( 'NONE', ( #4325 ), #325, .F. ) ;
#599 = DIRECTION ( 'NONE',  ( -1.000000000000000000, 0.000000000000000000, 0.000000000000000000 ) ) ;
#600 = PRODUCT_CONTEXT ( 'NONE', #768, 'mechanical' ) ;
#601 = EDGE_CURVE ( 'NONE', #4279, #3704, #1126, .T. ) ;
#602 = EDGE_LOOP ( 'NONE', ( #718, #4210, #661, #1411 ) ) ;
#603 = DIRECTION ( 'NONE',  ( -1.000000000000000000, 0.000000000000000000, 0.000000000000000000 ) ) ;
#604 = CARTESIAN_POINT ( 'NONE',  ( 15.00000000000000000, -11.80087472665740655, -21.71428571428571885 ) ) ;
#605 = CARTESIAN_POINT ( 'NONE',  ( 24.55500000000002103, 3.061616997868384620E-16, -2.500000000000001332 ) ) ;
#606 = ORIENTED_EDGE ( 'NONE', *, *, #4600, .T. ) ;
#607 = ORIENTED_EDGE ( 'NONE', *, *, #1884, .F. ) ;
#608 = DIRECTION ( 'NONE',  ( 0.000000000000000000, 0.000000000000000000, 1.000000000000000000 ) ) ;
#609 = APPLICATION_CONTEXT ( 'automotive_design' ) ;
#610 = DIRECTION ( 'NONE',  ( 0.5150380749100550437, 0.000000000000000000, -0.8571673007021117785 ) ) ;
#611 = DIRECTION ( 'NONE',  ( -1.000000000000000000, 0.000000000000000000, 0.000000000000000000 ) ) ;
#612 = EDGE_LOOP ( 'NONE', ( #60, #1655 ) ) ;
#613 = PRODUCT ( 'socket head cap screw_iso_ISO 4762 M4 x 20 - 20N', 'socket head cap screw_iso_ISO 4762 M4 x 20 - 20N', '', ( #3146 ) ) ;
#614 = DIRECTION ( 'NONE',  ( -1.000000000000000000, 0.000000000000000000, -0.000000000000000000 ) ) ;
#615 = DIRECTION ( 'NONE',  ( 0.000000000000000000, 0.000000000000000000, 1.000000000000000000 ) ) ;
#616 = ORIENTED_EDGE ( 'NONE', *, *, #3305, .T. ) ;
#617 = MECHANICAL_DESIGN_GEOMETRIC_PRESENTATION_REPRESENTATION (  '', ( #1267 ), #2875 ) ;
#618 = DIRECTION ( 'NONE',  ( -0.000000000000000000, -0.000000000000000000, 1.000000000000000000 ) ) ;
#619 = DIRECTION ( 'NONE',  ( -1.000000000000000000, -0.000000000000000000, -0.000000000000000000 ) ) ;
#620 = PRESENTATION_STYLE_ASSIGNMENT (( #4050 ) ) ;
#621 = ORIENTED_EDGE ( 'NONE', *, *, #2351, .F. ) ;
#622 = ADVANCED_FACE ( 'NONE', ( #3955 ), #3927, .F. ) ;
#623 = EDGE_CURVE ( 'NONE', #4219, #2953, #1516, .T. ) ;
#624 = LINE ( 'NONE', #3677, #576 ) ;
#625 = FACE_BOUND ( 'NONE', #874, .T. ) ;
#626 = LINE ( 'NONE', #4130, #2829 ) ;
#627 = ORIENTED_EDGE ( 'NONE', *, *, #2610, .F. ) ;
#628 = EDGE_CURVE ( 'NONE', #4218, #3494, #3207, .T. ) ;
#629 = CARTESIAN_POINT ( 'NONE',  ( 2.500000000000000000, 2.357898499370433054, -1.951563910473907981E-15 ) ) ;
#630 =( LENGTH_UNIT ( ) NAMED_UNIT ( * ) SI_UNIT ( .MILLI., .METRE. ) );
#631 = CIRCLE ( 'NONE', #3433, 25.00000000000000000 ) ;
#632 = DIRECTION ( 'NONE',  ( 0.000000000000000000, 0.000000000000000000, 1.000000000000000000 ) ) ;
#633 = CARTESIAN_POINT ( 'NONE',  ( -6.517431832507181422E-14, 16.00000000000000000, -28.10000000000000142 ) ) ;
#634 = DIRECTION ( 'NONE',  ( 1.000000000000000000, 0.000000000000000000, 0.000000000000000000 ) ) ;
#635 = ORIENTED_EDGE ( 'NONE', *, *, #379, .F. ) ;
#636 = FACE_BOUND ( 'NONE', #612, .T. ) ;
#637 = DIRECTION ( 'NONE',  ( 0.000000000000000000, 0.000000000000000000, -1.000000000000000000 ) ) ;
#638 = DIRECTION ( 'NONE',  ( 0.000000000000000000, 0.000000000000000000, 1.000000000000000000 ) ) ;
#639 = AXIS2_PLACEMENT_3D ( 'NONE', #2764, #2840, #2031 ) ;
#640 = ORIENTED_EDGE ( 'NONE', *, *, #4116, .T. ) ;
#641 = CIRCLE ( 'NONE', #2418, 4.250000000000000000 ) ;
#642 = CARTESIAN_POINT ( 'NONE',  ( -13.99999999999993250, -16.00000000000000000, -26.00000000000000355 ) ) ;
#643 = FACE_OUTER_BOUND ( 'NONE', #3434, .T. ) ;
#644 = AXIS2_PLACEMENT_3D ( 'NONE', #1689, #4751, #1713 ) ;
#645 = VERTEX_POINT ( 'NONE', #1974 ) ;
#646 = EDGE_CURVE ( 'NONE', #1680, #4219, #2359, .T. ) ;
#647 = VECTOR ( 'NONE', #648, 1000.000000000000000 ) ;
#648 = DIRECTION ( 'NONE',  ( -0.000000000000000000, -0.000000000000000000, 1.000000000000000000 ) ) ;
#649 = CYLINDRICAL_SURFACE ( 'NONE', #973, 6.999999999999999112 ) ;
#650 = CARTESIAN_POINT ( 'NONE',  ( 8.500000000000000000, -21.37171027316251681, 12.00000000000000000 ) ) ;
#651 = CIRCLE ( 'NONE', #978, 2.649999999999995914 ) ;
#652 = VECTOR ( 'NONE', #2590, 1000.000000000000000 ) ;
#653 = CIRCLE ( 'NONE', #3857, 2.099999999999997868 ) ;
#654 = VERTEX_POINT ( 'NONE', #4651 ) ;
#655 = EDGE_CURVE ( 'NONE', #2974, #2709, #2729, .T. ) ;
#656 = CARTESIAN_POINT ( 'NONE',  ( 2.500000000000000000, -2.357898499370432610, 3.252606517456513302E-15 ) ) ;
#657 = CONICAL_SURFACE ( 'NONE', #3947, 2.055000000000000160, 0.7853981633974721488 ) ;
#658 = PLANE ( 'NONE',  #2178 ) ;
#659 = AXIS2_PLACEMENT_3D ( 'NONE', #1459, #3001, #4158 ) ;
#660 = FACE_OUTER_BOUND ( 'NONE', #1788, .T. ) ;
#661 = ORIENTED_EDGE ( 'NONE', *, *, #3804, .T. ) ;
#662 = CARTESIAN_POINT ( 'NONE',  ( 4.000000000000003553, 0.000000000000000000, 0.000000000000000000 ) ) ;
#663 = ORIENTED_EDGE ( 'NONE', *, *, #1176, .T. ) ;
#664 = EDGE_CURVE ( 'NONE', #1044, #571, #3133, .T. ) ;
#665 = ORIENTED_EDGE ( 'NONE', *, *, #2003, .T. ) ;
#666 = AXIS2_PLACEMENT_3D ( 'NONE', #4115, #686, #239 ) ;
#667 = LINE ( 'NONE', #3029, #2342 ) ;
#668 = DIRECTION ( 'NONE',  ( 1.000000000000000000, 0.000000000000000000, 0.000000000000000000 ) ) ;
#669 = DIRECTION ( 'NONE',  ( 0.000000000000000000, 0.000000000000000000, 1.000000000000000000 ) ) ;
#670 = AXIS2_PLACEMENT_3D ( 'NONE', #3868, #3890, #1940 ) ;
#671 = ORIENTED_EDGE ( 'NONE', *, *, #1694, .T. ) ;
#672 = CARTESIAN_POINT ( 'NONE',  ( 0.000000000000000000, -25.00000000000000000, -32.00000000000000000 ) ) ;
#673 = CYLINDRICAL_SURFACE ( 'NONE', #4506, 1.000000000000000888 ) ;
#674 = COLOUR_RGB ( '', 0.09019608, 0.27058824, 0.51372549) ;
#675 = VERTEX_POINT ( 'NONE', #218 ) ;
#676 = DIRECTION ( 'NONE',  ( -1.000000000000000000, -0.000000000000000000, -0.000000000000000000 ) ) ;
#677 = DIRECTION ( 'NONE',  ( 0.000000000000000000, 0.000000000000000000, 1.000000000000000000 ) ) ;
#678 = CARTESIAN_POINT ( 'NONE',  ( -12.50000000000000178, 19.30673457630782863, 12.00000000000000000 ) ) ;
#679 = ORIENTED_EDGE ( 'NONE', *, *, #1273, .F. ) ;
#680 = ORIENTED_EDGE ( 'NONE', *, *, #2473, .T. ) ;
#681 = SURFACE_STYLE_FILL_AREA ( #2969 ) ;
#682 = CARTESIAN_POINT ( 'NONE',  ( 25.00000000000000000, 0.000000000000000000, 0.000000000000000000 ) ) ;
#683 = CARTESIAN_POINT ( 'NONE',  ( -3.041771206386918902E-14, -8.500000000000001776, -4.000000000000000000 ) ) ;
#684 = EDGE_CURVE ( 'NONE', #2597, #4218, #190, .T. ) ;
#685 = ORIENTED_EDGE ( 'NONE', *, *, #4356, .F. ) ;
#686 = DIRECTION ( 'NONE',  ( 0.000000000000000000, 0.8660254037844381525, -0.5000000000000009992 ) ) ;
#687 = ORIENTED_EDGE ( 'NONE', *, *, #2074, .F. ) ;
#688 = LINE ( 'NONE', #3368, #510 ) ;
#689 = CARTESIAN_POINT ( 'NONE',  ( 16.10609822396473589, 5.440000000000003055, -4.000000000000000000 ) ) ;
#690 = EDGE_CURVE ( 'NONE', #4023, #3361, #4322, .T. ) ;
#691 = DIRECTION ( 'NONE',  ( -1.000000000000000000, 0.000000000000000000, 0.000000000000000000 ) ) ;
#692 = EDGE_CURVE ( 'NONE', #4023, #675, #2130, .T. ) ;
#693 = ORIENTED_EDGE ( 'NONE', *, *, #4446, .T. ) ;
#694 = DIRECTION ( 'NONE',  ( 0.000000000000000000, 0.000000000000000000, -1.000000000000000000 ) ) ;
#695 =( LENGTH_UNIT ( ) NAMED_UNIT ( * ) SI_UNIT ( .MILLI., .METRE. ) );
#696 = CARTESIAN_POINT ( 'NONE',  ( 0.000000000000000000, 0.000000000000000000, -20.00000000000000000 ) ) ;
#697 = ORIENTED_EDGE ( 'NONE', *, *, #53, .T. ) ;
#698 = CARTESIAN_POINT ( 'NONE',  ( 2.444036937190193033E-14, 6.999999999999999112, -20.00000000000000000 ) ) ;
#699 = FACE_BOUND ( 'NONE', #2377, .T. ) ;
#700 = CARTESIAN_POINT ( 'NONE',  ( 2.500000000000000000, 0.000000000000000000, 0.000000000000000000 ) ) ;
#701 = ORIENTED_EDGE ( 'NONE', *, *, #4533, .T. ) ;
#702 = ORIENTED_EDGE ( 'NONE', *, *, #3113, .T. ) ;
#703 = CARTESIAN_POINT ( 'NONE',  ( 4.199999999999995737, 2.694222958124178486E-16, 2.200000000000001066 ) ) ;
#704 = CARTESIAN_POINT ( 'NONE',  ( 2.000000000000000000, 1.773042676681340968, -2.276824562219559311E-15 ) ) ;
#705 = CARTESIAN_POINT ( 'NONE',  ( 0.000000000000000000, 25.00000000000000000, -32.00000000000000000 ) ) ;
#706 = ORIENTED_EDGE ( 'NONE', *, *, #4609, .F. ) ;
#707 = ORIENTED_EDGE ( 'NONE', *, *, #765, .F. ) ;
#708 = EDGE_CURVE ( 'NONE', #2396, #2782, #2504, .T. ) ;
#709 = EDGE_CURVE ( 'NONE', #297, #4462, #2906, .T. ) ;
#710 = DIRECTION ( 'NONE',  ( 0.000000000000000000, 0.000000000000000000, 1.000000000000000000 ) ) ;
#711 = CARTESIAN_POINT ( 'NONE',  ( 0.000000000000000000, 0.000000000000000000, -20.00000000000000000 ) ) ;
#712 =( NAMED_UNIT ( * ) SI_UNIT ( $, .STERADIAN. ) SOLID_ANGLE_UNIT ( ) );
#713 = AXIS2_PLACEMENT_3D ( 'NONE', #1995, #4324, #507 ) ;
#714 = ORIENTED_EDGE ( 'NONE', *, *, #623, .F. ) ;
#715 = EDGE_CURVE ( 'NONE', #2919, #4243, #4022, .T. ) ;
#716 = DIRECTION ( 'NONE',  ( 0.000000000000000000, -0.5000000000000011102, -0.8660254037844379305 ) ) ;
#717 = CARTESIAN_POINT ( 'NONE',  ( -19.30673457630776824, 12.50000000000006750, -12.00000000000000000 ) ) ;
#718 = ORIENTED_EDGE ( 'NONE', *, *, #4825, .T. ) ;
#719 = ADVANCED_FACE ( 'NONE', ( #2078 ), #1718, .F. ) ;
#720 = VECTOR ( 'NONE', #1698, 1000.000000000000000 ) ;
#721 = DIRECTION ( 'NONE',  ( 0.000000000000000000, 0.000000000000000000, 1.000000000000000000 ) ) ;
#722 = VECTOR ( 'NONE', #786, 1000.000000000000000 ) ;
#723 = CARTESIAN_POINT ( 'NONE',  ( -9.000000000000003553, -1.999999999999999112, -32.00000000000000000 ) ) ;
#724 = CARTESIAN_POINT ( 'NONE',  ( 6.497531322021036645E-14, -16.00000000000000000, -23.90000000000000568 ) ) ;
#725 = FACE_OUTER_BOUND ( 'NONE', #235, .T. ) ;
#726 = ORIENTED_EDGE ( 'NONE', *, *, #4181, .T. ) ;
#727 = AXIS2_PLACEMENT_3D ( 'NONE', #2613, #3752, #4129 ) ;
#728 = AXIS2_PLACEMENT_3D ( 'NONE', #4369, #3714, #4113 ) ;
#729 = ORIENTED_EDGE ( 'NONE', *, *, #2155, .T. ) ;
#730 = DIRECTION ( 'NONE',  ( 0.000000000000000000, 0.000000000000000000, -1.000000000000000000 ) ) ;
#731 = DIRECTION ( 'NONE',  ( -0.000000000000000000, -0.000000000000000000, 1.000000000000000000 ) ) ;
#732 = AXIS2_PLACEMENT_3D ( 'NONE', #1683, #1380, #2536 ) ;
#733 = LINE ( 'NONE', #3464, #4106 ) ;
#734 = AXIS2_PLACEMENT_3D ( 'NONE', #2871, #2065, #2419 ) ;
#735 = EDGE_LOOP ( 'NONE', ( #2699, #2041, #219, #517, #2538 ) ) ;
#736 = EDGE_LOOP ( 'NONE', ( #292, #543, #3161, #69, #606 ) ) ;
#737 = AXIS2_PLACEMENT_3D ( 'NONE', #2501, #946, #4021 ) ;
#738 = VECTOR ( 'NONE', #1161, 1000.000000000000000 ) ;
#739 = AXIS2_PLACEMENT_3D ( 'NONE', #742, #763, #391 ) ;
#740 = DIRECTION ( 'NONE',  ( -2.036697447658493800E-15, 1.000000000000000000, 0.000000000000000000 ) ) ;
#741 = CARTESIAN_POINT ( 'NONE',  ( -9.000000000000003553, -1.999999999999999112, -12.00000000000000000 ) ) ;
#742 = CARTESIAN_POINT ( 'NONE',  ( -31.74999999999995737, 0.000000000000000000, 0.000000000000000000 ) ) ;
#743 = VECTOR ( 'NONE', #4151, 1000.000000000000000 ) ;
#744 = ORIENTED_EDGE ( 'NONE', *, *, #487, .T. ) ;
#745 = AXIS2_PLACEMENT_3D ( 'NONE', #2471, #215, #119 ) ;
#746 = EDGE_CURVE ( 'NONE', #2092, #2240, #994, .T. ) ;
#747 = ORIENTED_EDGE ( 'NONE', *, *, #1982, .F. ) ;
#748 = CARTESIAN_POINT ( 'NONE',  ( 22.31144310522464735, -11.28096319364321509, -29.72586080439007006 ) ) ;
#749 = EDGE_CURVE ( 'NONE', #1695, #3657, #3997, .T. ) ;
#750 = CARTESIAN_POINT ( 'NONE',  ( 0.000000000000000000, 0.000000000000000000, -12.00000000000000000 ) ) ;
#751 = EDGE_CURVE ( 'NONE', #1504, #3948, #2245, .T. ) ;
#752 = DIRECTION ( 'NONE',  ( -1.000000000000000000, 0.000000000000000000, 0.000000000000000000 ) ) ;
#753 = CARTESIAN_POINT ( 'NONE',  ( -8.500000000000001776, -9.407539813567788568E-16, 12.00000000000000000 ) ) ;
#754 = VERTEX_POINT ( 'NONE', #3235 ) ;
#755 = ADVANCED_BREP_SHAPE_REPRESENTATION ( '', ( #2079, #1918 ), #1581 ) ;
#756 = CARTESIAN_POINT ( 'NONE',  ( 21.37171027316252747, 8.499999999999930722, -12.00000000000000000 ) ) ;
#757 = CARTESIAN_POINT ( 'NONE',  ( 0.000000000000000000, -1.999999999999999112, -20.00000000000000000 ) ) ;
#758 = CYLINDRICAL_SURFACE ( 'NONE', #3930, 2.099999999999997868 ) ;
#759 = CARTESIAN_POINT ( 'NONE',  ( 21.97815564317848924, 11.91494984865602191, -31.58906108478248953 ) ) ;
#760 = ORIENTED_EDGE ( 'NONE', *, *, #4860, .T. ) ;
#761 = EDGE_LOOP ( 'NONE', ( #2798, #4883, #1651, #3117 ) ) ;
#762 = DIRECTION ( 'NONE',  ( 1.000000000000000000, -0.000000000000000000, -0.000000000000000000 ) ) ;
#763 = DIRECTION ( 'NONE',  ( -1.000000000000000000, -0.000000000000000000, -0.000000000000000000 ) ) ;
#764 = ORIENTED_EDGE ( 'NONE', *, *, #4789, .T. ) ;
#765 = EDGE_CURVE ( 'NONE', #148, #1558, #1764, .T. ) ;
#766 = CARTESIAN_POINT ( 'NONE',  ( 2.853620410115562697E-14, 8.500000000000001776, -12.00000000000000000 ) ) ;
#767 = DIRECTION ( 'NONE',  ( 1.000000000000000000, 0.000000000000000000, -0.000000000000000000 ) ) ;
#768 = APPLICATION_CONTEXT ( 'automotive_design' ) ;
#769 = ORIENTED_EDGE ( 'NONE', *, *, #2998, .T. ) ;
#770 = EDGE_LOOP ( 'NONE', ( #2887, #775 ) ) ;
#771 = CARTESIAN_POINT ( 'NONE',  ( -25.00000000000000000, 3.061616997868383043E-15, -12.00000000000000000 ) ) ;
#772 = DIRECTION ( 'NONE',  ( -1.000000000000000000, -0.000000000000000000, -0.000000000000000000 ) ) ;
#773 = CARTESIAN_POINT ( 'NONE',  ( 0.000000000000000000, -1.178949249685213863, 2.042000000000002924 ) ) ;
#774 = CARTESIAN_POINT ( 'NONE',  ( 2.500000000000000000, 2.357898499370433054, -1.951563910473907981E-15 ) ) ;
#775 = ORIENTED_EDGE ( 'NONE', *, *, #1417, .F. ) ;
#776 = EDGE_CURVE ( 'NONE', #313, #1525, #1394, .T. ) ;
#777 = MECHANICAL_DESIGN_GEOMETRIC_PRESENTATION_REPRESENTATION (  '', ( #4945 ), #4454 ) ;
#778 = CARTESIAN_POINT ( 'NONE',  ( 2.500000000000000000, -1.178949249685213863, 2.042000000000002924 ) ) ;
#779 = CARTESIAN_POINT ( 'NONE',  ( -10.00000000000002132, 16.00000000000000000, -26.00000000000000355 ) ) ;
#780 = CARTESIAN_POINT ( 'NONE',  ( -10.00000000000002132, 16.00000000000000000, -26.00000000000000355 ) ) ;
#781 = CARTESIAN_POINT ( 'NONE',  ( 22.04753367391286645, -11.78607713658132994, -20.26503649943386876 ) ) ;
#782 = ORIENTED_EDGE ( 'NONE', *, *, #2643, .T. ) ;
#783 = ADVANCED_FACE ( 'NONE', ( #569 ), #3598, .T. ) ;
#784 = ADVANCED_FACE ( 'NONE', ( #4441 ), #2889, .F. ) ;
#785 = ORIENTED_EDGE ( 'NONE', *, *, #1577, .T. ) ;
#786 = DIRECTION ( 'NONE',  ( 0.000000000000000000, -1.000000000000000000, 9.783878858594330870E-16 ) ) ;
#787 = FILL_AREA_STYLE ('',( #1511 ) ) ;
#788 = CYLINDRICAL_SURFACE ( 'NONE', #4749, 2.099999999999994316 ) ;
#789 = ORIENTED_EDGE ( 'NONE', *, *, #1903, .F. ) ;
#790 = UNCERTAINTY_MEASURE_WITH_UNIT (LENGTH_MEASURE( 1.000000000000000082E-05 ), #921, 'distance_accuracy_value', 'NONE');
#791 = CARTESIAN_POINT ( 'NONE',  ( 2.172477277502393807E-14, -16.00000000000000000, -28.09999999999999787 ) ) ;
#792 = DIRECTION ( 'NONE',  ( -0.000000000000000000, -0.000000000000000000, 1.000000000000000000 ) ) ;
#793 = AXIS2_PLACEMENT_3D ( 'NONE', #568, #872, #200 ) ;
#794 = ORIENTED_EDGE ( 'NONE', *, *, #3305, .F. ) ;
#795 = ORIENTED_EDGE ( 'NONE', *, *, #4142, .T. ) ;
#796 = VECTOR ( 'NONE', #2151, 1000.000000000000000 ) ;
#797 = CARTESIAN_POINT ( 'NONE',  ( 22.87614623887219167, 10.08384657499285808, -24.98007506026046798 ) ) ;
#798 = DIRECTION ( 'NONE',  ( 0.000000000000000000, 0.000000000000000000, 1.000000000000000000 ) ) ;
#799 = DIRECTION ( 'NONE',  ( -0.7071067811865359154, 8.659560562355074607E-17, -0.7071067811865591191 ) ) ;
#800 = EDGE_CURVE ( 'NONE', #3536, #4716, #4237, .T. ) ;
#801 = AXIS2_PLACEMENT_3D ( 'NONE', #2152, #4779, #1345 ) ;
#802 = EDGE_CURVE ( 'NONE', #1443, #1649, #1414, .T. ) ;
#803 = VERTEX_POINT ( 'NONE', #2455 ) ;
#804 = AXIS2_PLACEMENT_3D ( 'NONE', #1991, #1195, #3919 ) ;
#805 = DIRECTION ( 'NONE',  ( 1.000000000000000000, 0.000000000000000000, 0.000000000000000000 ) ) ;
#806 = DIRECTION ( 'NONE',  ( -0.000000000000000000, -0.000000000000000000, 1.000000000000000000 ) ) ;
#807 = CARTESIAN_POINT ( 'NONE',  ( 21.88691174701116182, -12.08152700620045117, -20.77757659040560512 ) ) ;
#808 = EDGE_CURVE ( 'NONE', #4311, #4747, #3622, .T. ) ;
#809 = VECTOR ( 'NONE', #2774, 1000.000000000000000 ) ;
#810 = CIRCLE ( 'NONE', #1521, 2.649999999999985700 ) ;
#811 = VERTEX_POINT ( 'NONE', #4516 ) ;
#812 = PRODUCT_DEFINITION_SHAPE ( 'NONE', 'NONE',  #596 ) ;
#813 = ORIENTED_EDGE ( 'NONE', *, *, #4024, .F. ) ;
#814 = FILL_AREA_STYLE ('',( #4620 ) ) ;
#815 = CIRCLE ( 'NONE', #1850, 2.099999999999997868 ) ;
#816 = DIRECTION ( 'NONE',  ( 0.5150380749100544886, 1.049727191138618449E-16, 0.8571673007021121116 ) ) ;
#817 = AXIS2_PLACEMENT_3D ( 'NONE', #383, #3437, #1166 ) ;
#818 = LINE ( 'NONE', #117, #4015 ) ;
#819 = DIRECTION ( 'NONE',  ( 0.000000000000000000, 0.000000000000000000, 1.000000000000000000 ) ) ;
#820 = EDGE_CURVE ( 'NONE', #4459, #803, #4874, .T. ) ;
#821 = ORIENTED_EDGE ( 'NONE', *, *, #3902, .T. ) ;
#822 = VECTOR ( 'NONE', #3608, 1000.000000000000114 ) ;
#823 =( GEOMETRIC_REPRESENTATION_CONTEXT ( 3 ) GLOBAL_UNCERTAINTY_ASSIGNED_CONTEXT ( ( #1800 ) ) GLOBAL_UNIT_ASSIGNED_CONTEXT ( ( #4904, #2244, #712 ) ) REPRESENTATION_CONTEXT ( 'NONE', 'WORKASPACE' ) );
#824 = CARTESIAN_POINT ( 'NONE',  ( 0.000000000000000000, 0.000000000000000000, 0.000000000000000000 ) ) ;
#825 = DIRECTION ( 'NONE',  ( 0.000000000000000000, 0.000000000000000000, -1.000000000000000000 ) ) ;
#826 = AXIS2_PLACEMENT_3D ( 'NONE', #4881, #4295, #1197 ) ;
#827 = ORIENTED_EDGE ( 'NONE', *, *, #2659, .T. ) ;
#828 = EDGE_LOOP ( 'NONE', ( #2198, #680, #835, #671, #2741 ) ) ;
#829 = CIRCLE ( 'NONE', #1462, 4.250000000000000000 ) ;
#830 = UNCERTAINTY_MEASURE_WITH_UNIT (LENGTH_MEASURE( 1.000000000000000082E-05 ), #3517, 'distance_accuracy_value', 'NONE');
#831 = CARTESIAN_POINT ( 'NONE',  ( 22.91733099102425442, 9.989778831080645460, -25.99421712970024245 ) ) ;
#832 = DIRECTION ( 'NONE',  ( 1.000000000000000000, 0.000000000000000000, 0.000000000000000000 ) ) ;
#833 = DIRECTION ( 'NONE',  ( 0.000000000000000000, 0.000000000000000000, 1.000000000000000000 ) ) ;
#834 = ORIENTED_EDGE ( 'NONE', *, *, #848, .T. ) ;
#835 = ORIENTED_EDGE ( 'NONE', *, *, #3508, .T. ) ;
#836 = VECTOR ( 'NONE', #2616, 1000.000000000000000 ) ;
#837 = ITEM_DEFINED_TRANSFORMATION ( 'NONE', 'NONE', #1106,  #1918 ) ;
#838 = CARTESIAN_POINT ( 'NONE',  ( -31.74999999999995737, 4.286263797015736595E-16, -3.500000000000000000 ) ) ;
#839 = LINE ( 'NONE', #2341, #3531 ) ;
#840 = CARTESIAN_POINT ( 'NONE',  ( 21.87320774003119794, -12.10631999347636345, -20.98456915527629363 ) ) ;
#841 = VECTOR ( 'NONE', #3213, 1000.000000000000000 ) ;
#842 = ORIENTED_EDGE ( 'NONE', *, *, #1820, .T. ) ;
#843 = ORIENTED_EDGE ( 'NONE', *, *, #4547, .T. ) ;
#844 = DIRECTION ( 'NONE',  ( 1.000000000000000000, -0.000000000000000000, -0.000000000000000000 ) ) ;
#845 = CARTESIAN_POINT ( 'NONE',  ( 0.000000000000000000, 0.000000000000000000, 4.000000000000000000 ) ) ;
#846 = CARTESIAN_POINT ( 'NONE',  ( 25.00000000000000000, 3.061616997868383043E-15, 2.000000000000001776 ) ) ;
#847 = ORIENTED_EDGE ( 'NONE', *, *, #133, .T. ) ;
#848 = EDGE_CURVE ( 'NONE', #3754, #468, #3922, .T. ) ;
#849 = EDGE_CURVE ( 'NONE', #1731, #4866, #1094, .T. ) ;
#850 = LINE ( 'NONE', #4216, #4959 ) ;
#851 = FACE_OUTER_BOUND ( 'NONE', #2534, .T. ) ;
#852 = VERTEX_POINT ( 'NONE', #2573 ) ;
#853 = PRODUCT ( 'Input Clamping Hub Sleeve', 'Input Clamping Hub Sleeve', '', ( #574 ) ) ;
#854 = EDGE_LOOP ( 'NONE', ( #2425, #1849, #2892, #2036 ) ) ;
#855 = CARTESIAN_POINT ( 'NONE',  ( 22.52717933085839874, -10.84147272832753472, -22.92928814334748466 ) ) ;
#856 = SURFACE_SIDE_STYLE ('',( #2768 ) ) ;
#857 = LINE ( 'NONE', #3094, #4406 ) ;
#858 = ORIENTED_EDGE ( 'NONE', *, *, #1121, .F. ) ;
#859 = ORIENTED_EDGE ( 'NONE', *, *, #3629, .T. ) ;
#860 = APPLICATION_PROTOCOL_DEFINITION ( 'draft international standard', 'automotive_design', 1998, #938 ) ;
#861 = DIRECTION ( 'NONE',  ( 1.000000000000000000, 0.000000000000000000, 0.000000000000000000 ) ) ;
#862 = FACE_OUTER_BOUND ( 'NONE', #1009, .T. ) ;
#863 = LINE ( 'NONE', #188, #4336 ) ;
#864 = ORIENTED_EDGE ( 'NONE', *, *, #3599, .F. ) ;
#865 = VERTEX_POINT ( 'NONE', #3009 ) ;
#866 = LINE ( 'NONE', #2374, #1925 ) ;
#867 = DIRECTION ( 'NONE',  ( 1.000000000000000000, -0.000000000000000000, -0.000000000000000000 ) ) ;
#868 = CARTESIAN_POINT ( 'NONE',  ( 0.000000000000000000, 0.000000000000000000, 0.000000000000000000 ) ) ;
#869 = EDGE_CURVE ( 'NONE', #4351, #2929, #1287, .T. ) ;
#870 = EDGE_CURVE ( 'NONE', #2692, #3603, #4723, .T. ) ;
#871 = ORIENTED_EDGE ( 'NONE', *, *, #3110, .F. ) ;
#872 = DIRECTION ( 'NONE',  ( -0.000000000000000000, -0.000000000000000000, -1.000000000000000000 ) ) ;
#873 = CARTESIAN_POINT ( 'NONE',  ( 0.000000000000000000, 0.000000000000000000, -20.00000000000000000 ) ) ;
#874 = EDGE_LOOP ( 'NONE', ( #4323, #3014, #1256, #4847, #349 ) ) ;
#875 = ORIENTED_EDGE ( 'NONE', *, *, #1061, .F. ) ;
#876 = VECTOR ( 'NONE', #716, 1000.000000000000114 ) ;
#877 = CARTESIAN_POINT ( 'NONE',  ( 0.000000000000000000, -1.178949249685218303, -2.041999999999998039 ) ) ;
#878 = CARTESIAN_POINT ( 'NONE',  ( 15.00000000000000000, -11.10102051443364068, -32.00000000000000000 ) ) ;
#879 = DIRECTION ( 'NONE',  ( 0.000000000000000000, -1.000000000000000000, 1.471414886128461471E-15 ) ) ;
#880 = EDGE_CURVE ( 'NONE', #3891, #4613, #1042, .T. ) ;
#881 = VERTEX_POINT ( 'NONE', #3443 ) ;
#882 = AXIS2_PLACEMENT_3D ( 'NONE', #3346, #4515, #1738 ) ;
#883 = ORIENTED_EDGE ( 'NONE', *, *, #3777, .F. ) ;
#884 = DIRECTION ( 'NONE',  ( 0.000000000000000000, 0.000000000000000000, -1.000000000000000000 ) ) ;
#885 = CARTESIAN_POINT ( 'NONE',  ( 25.00000000000000000, -11.10102051443364424, -21.00000000000000000 ) ) ;
#886 = DIRECTION ( 'NONE',  ( -1.106769389831504682E-16, 1.000000000000000000, 0.000000000000000000 ) ) ;
#887 = EDGE_LOOP ( 'NONE', ( #157, #875 ) ) ;
#888 = AXIS2_PLACEMENT_3D ( 'NONE', #1755, #1321, #140 ) ;
#889 = ORIENTED_EDGE ( 'NONE', *, *, #3864, .F. ) ;
#890 = CARTESIAN_POINT ( 'NONE',  ( 15.00000000000000000, 11.10102051443364068, -31.00000000000000000 ) ) ;
#891 = CARTESIAN_POINT ( 'NONE',  ( 0.000000000000000000, 0.000000000000000000, -12.00000000000000000 ) ) ;
#892 = AXIS2_PLACEMENT_3D ( 'NONE', #2942, #989, #2146 ) ;
#893 = DIRECTION ( 'NONE',  ( 0.000000000000000000, 0.000000000000000000, 1.000000000000000000 ) ) ;
#894 = VERTEX_POINT ( 'NONE', #741 ) ;
#895 = AXIS2_PLACEMENT_3D ( 'NONE', #2335, #3116, #879 ) ;
#896 = AXIS2_PLACEMENT_3D ( 'NONE', #1494, #676, #721 ) ;
#897 = DIRECTION ( 'NONE',  ( -0.000000000000000000, -0.000000000000000000, -1.000000000000000000 ) ) ;
#898 = EDGE_CURVE ( 'NONE', #3704, #1580, #4887, .T. ) ;
#899 = DIRECTION ( 'NONE',  ( 0.000000000000000000, 0.000000000000000000, -1.000000000000000000 ) ) ;
#900 = AXIS2_PLACEMENT_3D ( 'NONE', #1114, #4163, #1487 ) ;
#901 = VECTOR ( 'NONE', #135, 1000.000000000000000 ) ;
#902 = CIRCLE ( 'NONE', #1617, 1.610000000000000098 ) ;
#903 = ORIENTED_EDGE ( 'NONE', *, *, #1204, .T. ) ;
#904 = ADVANCED_FACE ( 'NONE', ( #2625 ), #296, .F. ) ;
#905 = CARTESIAN_POINT ( 'NONE',  ( 23.68543856465402442, -8.000000000000003553, -4.000000000000000000 ) ) ;
#906 = AXIS2_PLACEMENT_3D ( 'NONE', #1992, #422, #1970 ) ;
#907 = EDGE_CURVE ( 'NONE', #553, #1430, #4192, .T. ) ;
#908 = PRESENTATION_STYLE_ASSIGNMENT (( #2061 ) ) ;
#909 = PLANE ( 'NONE',  #2835 ) ;
#910 = LINE ( 'NONE', #1678, #1139 ) ;
#911 = EDGE_LOOP ( 'NONE', ( #4750, #2184, #415, #388 ) ) ;
#912 = ORIENTED_EDGE ( 'NONE', *, *, #4390, .F. ) ;
#913 = EDGE_CURVE ( 'NONE', #4443, #3659, #2973, .T. ) ;
#914 = ADVANCED_FACE ( 'NONE', ( #4098 ), #1509, .T. ) ;
#915 = VECTOR ( 'NONE', #4018, 1000.000000000000000 ) ;
#916 = DIRECTION ( 'NONE',  ( 0.000000000000000000, 0.000000000000000000, -1.000000000000000000 ) ) ;
#917 = FACE_OUTER_BOUND ( 'NONE', #4676, .T. ) ;
#918 = CARTESIAN_POINT ( 'NONE',  ( 25.00000000000000000, 11.10102051443364068, -31.00000000000000000 ) ) ;
#919 = ORIENTED_EDGE ( 'NONE', *, *, #1536, .F. ) ;
#920 = ORIENTED_EDGE ( 'NONE', *, *, #3837, .F. ) ;
#921 =( LENGTH_UNIT ( ) NAMED_UNIT ( * ) SI_UNIT ( .MILLI., .METRE. ) );
#922 = DIRECTION ( 'NONE',  ( 0.000000000000000000, 1.000000000000000000, -1.467581828789149532E-15 ) ) ;
#923 = FACE_OUTER_BOUND ( 'NONE', #3338, .T. ) ;
#924 = VECTOR ( 'NONE', #3089, 1000.000000000000000 ) ;
#925 = DIRECTION ( 'NONE',  ( 0.000000000000000000, 0.000000000000000000, 1.000000000000000000 ) ) ;
#926 = ORIENTED_EDGE ( 'NONE', *, *, #2599, .T. ) ;
#927 = CARTESIAN_POINT ( 'NONE',  ( -9.000000000000003553, -1.999999999999999112, -12.00000000000000000 ) ) ;
#928 = DIRECTION ( 'NONE',  ( 0.000000000000000000, 0.000000000000000000, 1.000000000000000000 ) ) ;
#929 = ORIENTED_EDGE ( 'NONE', *, *, #746, .F. ) ;
#930 = EDGE_CURVE ( 'NONE', #153, #1150, #1071, .T. ) ;
#931 = LINE ( 'NONE', #2457, #3169 ) ;
#932 = LINE ( 'NONE', #3978, #3232 ) ;
#933 = EDGE_LOOP ( 'NONE', ( #1425, #3642, #1924, #2330 ) ) ;
#934 = VERTEX_POINT ( 'NONE', #2604 ) ;
#935 = CARTESIAN_POINT ( 'NONE',  ( 0.000000000000000000, 0.000000000000000000, -20.00000000000000000 ) ) ;
#936 = CARTESIAN_POINT ( 'NONE',  ( 12.50000000000000178, 19.30673457630782863, 12.00000000000000000 ) ) ;
#937 = LINE ( 'NONE', #3914, #2427 ) ;
#938 = APPLICATION_CONTEXT ( 'automotive_design' ) ;
#939 = EDGE_CURVE ( 'NONE', #1050, #216, #4903, .T. ) ;
#940 = ORIENTED_EDGE ( 'NONE', *, *, #4943, .T. ) ;
#941 = VERTEX_POINT ( 'NONE', #369 ) ;
#942 = LINE ( 'NONE', #213, #4561 ) ;
#943 = CARTESIAN_POINT ( 'NONE',  ( 25.00000000000000000, 0.000000000000000000, -20.00000000000000000 ) ) ;
#944 = CARTESIAN_POINT ( 'NONE',  ( 0.000000000000000000, 0.000000000000000000, -1.999999999999994893 ) ) ;
#945 = ORIENTED_EDGE ( 'NONE', *, *, #2751, .F. ) ;
#946 = DIRECTION ( 'NONE',  ( 1.000000000000000000, -0.000000000000000000, -0.000000000000000000 ) ) ;
#947 = DIRECTION ( 'NONE',  ( -1.000000000000000000, -0.000000000000000000, -0.000000000000000000 ) ) ;
#948 = ORIENTED_EDGE ( 'NONE', *, *, #4220, .T. ) ;
#949 = DIRECTION ( 'NONE',  ( 1.000000000000000000, 0.000000000000000000, 0.000000000000000000 ) ) ;
#950 = PRODUCT_CONTEXT ( 'NONE', #1025, 'mechanical' ) ;
#951 = CARTESIAN_POINT ( 'NONE',  ( -6.537332342993324937E-14, 16.00000000000000000, -26.00000000000000355 ) ) ;
#952 = AXIS2_PLACEMENT_3D ( 'NONE', #1109, #1559, #2694 ) ;
#953 = ORIENTED_EDGE ( 'NONE', *, *, #646, .F. ) ;
#954 = ADVANCED_FACE ( 'NONE', ( #3053 ), #4556, .T. ) ;
#955 = DIRECTION ( 'NONE',  ( -1.000000000000000000, 0.000000000000000000, 0.000000000000000000 ) ) ;
#956 = FACE_OUTER_BOUND ( 'NONE', #441, .T. ) ;
#957 = AXIS2_PLACEMENT_3D ( 'NONE', #1468, #300, #2156 ) ;
#958 = FACE_OUTER_BOUND ( 'NONE', #3956, .T. ) ;
#959 = ORIENTED_EDGE ( 'NONE', *, *, #3343, .T. ) ;
#960 = ORIENTED_EDGE ( 'NONE', *, *, #1121, .T. ) ;
#961 = LINE ( 'NONE', #2493, #1519 ) ;
#962 = DIRECTION ( 'NONE',  ( 0.000000000000000000, 0.000000000000000000, -1.000000000000000000 ) ) ;
#963 = EDGE_CURVE ( 'NONE', #1731, #3126, #1842, .T. ) ;
#964 = EDGE_LOOP ( 'NONE', ( #3898, #1479, #2019, #627, #4843, #4193 ) ) ;
#965 = DIRECTION ( 'NONE',  ( 1.000000000000000000, 0.000000000000000000, 0.000000000000000000 ) ) ;
#966 = EDGE_CURVE ( 'NONE', #4690, #2597, #390, .T. ) ;
#967 = CARTESIAN_POINT ( 'NONE',  ( 21.97031423931356287, -11.92955703141274881, -31.59565500209243183 ) ) ;
#968 = CIRCLE ( 'NONE', #4077, 25.00000000000000000 ) ;
#969 = ORIENTED_EDGE ( 'NONE', *, *, #1204, .F. ) ;
#970 = CIRCLE ( 'NONE', #1609, 0.2000000000000000944 ) ;
#971 = FACE_OUTER_BOUND ( 'NONE', #761, .T. ) ;
#972 = PRODUCT_CONTEXT ( 'NONE', #2153, 'mechanical' ) ;
#973 = AXIS2_PLACEMENT_3D ( 'NONE', #3359, #2664, #1028 ) ;
#974 = CARTESIAN_POINT ( 'NONE',  ( 0.000000000000000000, 0.000000000000000000, -12.00000000000000000 ) ) ;
#975 = AXIS2_PLACEMENT_3D ( 'NONE', #1315, #3964, #538 ) ;
#976 =( LENGTH_UNIT ( ) NAMED_UNIT ( * ) SI_UNIT ( .MILLI., .METRE. ) );
#977 = ORIENTED_EDGE ( 'NONE', *, *, #4608, .F. ) ;
#978 = AXIS2_PLACEMENT_3D ( 'NONE', #2150, #2475, #2105 ) ;
#979 = AXIS2_PLACEMENT_3D ( 'NONE', #2447, #540, #3966 ) ;
#980 =( GEOMETRIC_REPRESENTATION_CONTEXT ( 3 ) GLOBAL_UNCERTAINTY_ASSIGNED_CONTEXT ( ( #3402 ) ) GLOBAL_UNIT_ASSIGNED_CONTEXT ( ( #4707, #1310, #204 ) ) REPRESENTATION_CONTEXT ( 'NONE', 'WORKASPACE' ) );
#981 = LINE ( 'NONE', #2853, #1772 ) ;
#982 = PLANE ( 'NONE',  #1299 ) ;
#983 = AXIS2_PLACEMENT_3D ( 'NONE', #1773, #1399, #2552 ) ;
#984 = LINE ( 'NONE', #4405, #3775 ) ;
#985 = ORIENTED_EDGE ( 'NONE', *, *, #2110, .T. ) ;
#986 = EDGE_CURVE ( 'NONE', #3389, #2431, #4002, .T. ) ;
#987 = VERTEX_POINT ( 'NONE', #1248 ) ;
#988 = DIRECTION ( 'NONE',  ( -1.000000000000000000, -0.000000000000000000, -0.000000000000000000 ) ) ;
#989 = DIRECTION ( 'NONE',  ( 1.000000000000000000, -0.000000000000000000, -0.000000000000000000 ) ) ;
#990 = FACE_OUTER_BOUND ( 'NONE', #3983, .T. ) ;
#991 = VERTEX_POINT ( 'NONE', #116 ) ;
#992 = CARTESIAN_POINT ( 'NONE',  ( 15.00000000000000000, -20.00000000000000355, -32.00000000000000000 ) ) ;
#993 = DIRECTION ( 'NONE',  ( 0.000000000000000000, 0.000000000000000000, -1.000000000000000000 ) ) ;
#994 = LINE ( 'NONE', #2477, #4000 ) ;
#995 = ORIENTED_EDGE ( 'NONE', *, *, #430, .T. ) ;
#996 = ADVANCED_BREP_SHAPE_REPRESENTATION ( '', ( #1999, #1918 ), #3816 ) ;
#997 = CIRCLE ( 'NONE', #1245, 22.99999999999998934 ) ;
#998 = ADVANCED_FACE ( 'NONE', ( #4621 ), #2428, .F. ) ;
#999 = ADVANCED_FACE ( 'NONE', ( #4643 ), #2652, .F. ) ;
#1000 = CARTESIAN_POINT ( 'NONE',  ( 16.10609822396473589, 5.440000000000003055, 14.30577747056276472 ) ) ;
#1001 = DIRECTION ( 'NONE',  ( 0.000000000000000000, 0.000000000000000000, -1.000000000000000000 ) ) ;
#1002 = APPLICATION_PROTOCOL_DEFINITION ( 'draft international standard', 'automotive_design', 1998, #3334 ) ;
#1003 = SURFACE_SIDE_STYLE ('',( #1916 ) ) ;
#1004 =( NAMED_UNIT ( * ) SI_UNIT ( $, .STERADIAN. ) SOLID_ANGLE_UNIT ( ) );
#1005 = ORIENTED_EDGE ( 'NONE', *, *, #430, .F. ) ;
#1006 = DIRECTION ( 'NONE',  ( 0.000000000000000000, 0.000000000000000000, 1.000000000000000000 ) ) ;
#1007 = CARTESIAN_POINT ( 'NONE',  ( -6.537332342993324937E-14, 16.00000000000000000, -26.00000000000000355 ) ) ;
#1008 = EDGE_LOOP ( 'NONE', ( #4046, #1246, #577 ) ) ;
#1009 = EDGE_LOOP ( 'NONE', ( #3602, #4092, #2424, #2514 ) ) ;
#1010 = DIRECTION ( 'NONE',  ( 1.000000000000000000, 0.000000000000000000, 0.000000000000000000 ) ) ;
#1011 = CARTESIAN_POINT ( 'NONE',  ( 24.00000000000000000, 2.210487472460972698E-16, -1.610000000000000098 ) ) ;
#1012 = LINE ( 'NONE', #2522, #2333 ) ;
#1013 = DIRECTION ( 'NONE',  ( -0.000000000000000000, -0.000000000000000000, -1.000000000000000000 ) ) ;
#1014 = ORIENTED_EDGE ( 'NONE', *, *, #1706, .T. ) ;
#1015 = FACE_OUTER_BOUND ( 'NONE', #3253, .T. ) ;
#1016 = PRODUCT ( 'Output Clamping Hub Sleeve', 'Output Clamping Hub Sleeve', '', ( #600 ) ) ;
#1017 = CYLINDRICAL_SURFACE ( 'NONE', #1512, 17.00000000000000000 ) ;
#1018 = DIRECTION ( 'NONE',  ( 0.000000000000000000, 0.000000000000000000, 1.000000000000000000 ) ) ;
#1019 = ADVANCED_FACE ( 'NONE', ( #1641 ), #3083, .T. ) ;
#1020 = EDGE_LOOP ( 'NONE', ( #1983, #557, #59, #4058, #714, #953 ) ) ;
#1021 = MECHANICAL_DESIGN_GEOMETRIC_PRESENTATION_REPRESENTATION (  '', ( #3423 ), #4138 ) ;
#1022 = CARTESIAN_POINT ( 'NONE',  ( 2.500000000000000000, 2.357898499370433054, -1.951563910473907981E-15 ) ) ;
#1023 = AXIS2_PLACEMENT_3D ( 'NONE', #2540, #4923, #31 ) ;
#1024 = VERTEX_POINT ( 'NONE', #4598 ) ;
#1025 = APPLICATION_CONTEXT ( 'automotive_design' ) ;
#1026 = CARTESIAN_POINT ( 'NONE',  ( 22.52496067886514197, 10.84608396733234592, -22.92156229269478374 ) ) ;
#1027 = EDGE_CURVE ( 'NONE', #3993, #1343, #968, .T. ) ;
#1028 = DIRECTION ( 'NONE',  ( 1.000000000000000000, 0.000000000000000000, 0.000000000000000000 ) ) ;
#1029 = PLANE ( 'NONE',  #4821 ) ;
#1030 = PRODUCT_DEFINITION_FORMATION_WITH_SPECIFIED_SOURCE ( 'ANY', '', #1374, .NOT_KNOWN. ) ;
#1031 = VERTEX_POINT ( 'NONE', #4319 ) ;
#1032 = PRESENTATION_STYLE_ASSIGNMENT (( #4012 ) ) ;
#1033 = TOROIDAL_SURFACE ( 'NONE', #1674, 2.200000000000001066, 0.2000000000000000111 ) ;
#1034 = CARTESIAN_POINT ( 'NONE',  ( 24.00000000000000000, 0.000000000000000000, 0.000000000000000000 ) ) ;
#1035 = DIRECTION ( 'NONE',  ( 1.000000000000000000, -0.000000000000000000, -0.000000000000000000 ) ) ;
#1036 = ORIENTED_EDGE ( 'NONE', *, *, #4737, .T. ) ;
#1037 = CARTESIAN_POINT ( 'NONE',  ( 5.000000000000004441, 0.000000000000000000, 0.000000000000000000 ) ) ;
#1038 = EDGE_LOOP ( 'NONE', ( #524, #589, #4148, #2680, #1210, #4780, #1790, #3348, #2804, #82 ) ) ;
#1039 =( GEOMETRIC_REPRESENTATION_CONTEXT ( 3 ) GLOBAL_UNCERTAINTY_ASSIGNED_CONTEXT ( ( #2653 ) ) GLOBAL_UNIT_ASSIGNED_CONTEXT ( ( #1392, #61, #3082 ) ) REPRESENTATION_CONTEXT ( 'NONE', 'WORKASPACE' ) );
#1040 = DIRECTION ( 'NONE',  ( -0.000000000000000000, -0.000000000000000000, 1.000000000000000000 ) ) ;
#1041 = DIRECTION ( 'NONE',  ( -0.000000000000000000, -0.000000000000000000, 1.000000000000000000 ) ) ;
#1042 = LINE ( 'NONE', #3766, #4728 ) ;
#1043 = CONICAL_SURFACE ( 'NONE', #1362, 2.099999999999997868, 1.029744258676654090 ) ;
#1044 = VERTEX_POINT ( 'NONE', #3873 ) ;
#1045 = AXIS2_PLACEMENT_3D ( 'NONE', #711, #2978, #4541 ) ;
#1046 = LINE ( 'NONE', #2578, #4876 ) ;
#1047 = DIRECTION ( 'NONE',  ( 1.000000000000000000, 0.000000000000000000, 0.000000000000000000 ) ) ;
#1048 = CIRCLE ( 'NONE', #433, 0.2000000000000000944 ) ;
#1049 = VECTOR ( 'NONE', #2565, 1000.000000000000114 ) ;
#1050 = VERTEX_POINT ( 'NONE', #1565 ) ;
#1051 = EDGE_CURVE ( 'NONE', #1467, #479, #3496, .T. ) ;
#1052 = AXIS2_PLACEMENT_3D ( 'NONE', #4364, #259, #3986 ) ;
#1053 = AXIS2_PLACEMENT_3D ( 'NONE', #974, #3260, #3214 ) ;
#1054 = LINE ( 'NONE', #2535, #2256 ) ;
#1055 = DIRECTION ( 'NONE',  ( 0.000000000000000000, 0.8660254037844380415, -0.5000000000000012212 ) ) ;
#1056 = PLANE ( 'NONE',  #1304 ) ;
#1057 = CIRCLE ( 'NONE', #2909, 23.00000000000000711 ) ;
#1058 = AXIS2_PLACEMENT_3D ( 'NONE', #3400, #2679, #251 ) ;
#1059 = VERTEX_POINT ( 'NONE', #501 ) ;
#1060 = EDGE_CURVE ( 'NONE', #3126, #4359, #2094, .T. ) ;
#1061 = EDGE_CURVE ( 'NONE', #1150, #2856, #327, .T. ) ;
#1062 = CIRCLE ( 'NONE', #3459, 23.00000000000000711 ) ;
#1063 = CARTESIAN_POINT ( 'NONE',  ( -16.10609822396473589, 5.440000000000003055, -4.000000000000000000 ) ) ;
#1064 = DIRECTION ( 'NONE',  ( 0.000000000000000000, 1.224646799147353207E-16, 1.000000000000000000 ) ) ;
#1065 = ORIENTED_EDGE ( 'NONE', *, *, #1116, .T. ) ;
#1066 = DIRECTION ( 'NONE',  ( 1.000000000000000000, -3.357200482488897685E-15, 0.000000000000000000 ) ) ;
#1067 = VERTEX_POINT ( 'NONE', #1221 ) ;
#1068 = CIRCLE ( 'NONE', #3623, 6.999999999999999112 ) ;
#1069 = CARTESIAN_POINT ( 'NONE',  ( 22.03949535914419755, -11.80087472665740655, -21.71428571428571885 ) ) ;
#1070 = CARTESIAN_POINT ( 'NONE',  ( 0.000000000000000000, 0.000000000000000000, -12.00000000000000000 ) ) ;
#1071 = LINE ( 'NONE', #2271, #2733 ) ;
#1072 = ORIENTED_EDGE ( 'NONE', *, *, #2379, .F. ) ;
#1073 = LINE ( 'NONE', #2182, #876 ) ;
#1074 = DIRECTION ( 'NONE',  ( 1.000000000000000000, 0.000000000000000000, 0.000000000000000000 ) ) ;
#1075 = CONTEXT_DEPENDENT_SHAPE_REPRESENTATION ( #2922, #1257 ) ;
#1076 = DIRECTION ( 'NONE',  ( 0.000000000000000000, 0.000000000000000000, -1.000000000000000000 ) ) ;
#1077 = AXIS2_PLACEMENT_3D ( 'NONE', #4425, #2866, #3670 ) ;
#1078 = ORIENTED_EDGE ( 'NONE', *, *, #1155, .T. ) ;
#1079 = CARTESIAN_POINT ( 'NONE',  ( 0.000000000000000000, 25.00000000000000000, -32.00000000000000000 ) ) ;
#1080 = CARTESIAN_POINT ( 'NONE',  ( 2.000000000000000000, 1.773042676681340968, -2.276824562219559311E-15 ) ) ;
#1081 = CARTESIAN_POINT ( 'NONE',  ( 22.40016391766193493, 11.10102051443364068, -32.00000000000000000 ) ) ;
#1082 = FACE_OUTER_BOUND ( 'NONE', #3709, .T. ) ;
#1083 = EDGE_LOOP ( 'NONE', ( #286, #4197, #170, #2268 ) ) ;
#1084 = DIRECTION ( 'NONE',  ( 0.000000000000000000, 0.000000000000000000, -1.000000000000000000 ) ) ;
#1085 = DIRECTION ( 'NONE',  ( 5.270590105383052810E-17, 1.742342977497177230E-17, -0.9999999999999998890 ) ) ;
#1086 = DIRECTION ( 'NONE',  ( 0.000000000000000000, 0.000000000000000000, 1.000000000000000000 ) ) ;
#1087 = FACE_OUTER_BOUND ( 'NONE', #1306, .T. ) ;
#1088 = CARTESIAN_POINT ( 'NONE',  ( -19.30673457630785350, -12.49999999999993250, -4.000000000000000000 ) ) ;
#1089 = EDGE_CURVE ( 'NONE', #3611, #3692, #4672, .T. ) ;
#1090 = ORIENTED_EDGE ( 'NONE', *, *, #3059, .T. ) ;
#1091 = ORIENTED_EDGE ( 'NONE', *, *, #1784, .T. ) ;
#1092 = CYLINDRICAL_SURFACE ( 'NONE', #900, 6.999999999999999112 ) ;
#1093 = DIRECTION ( 'NONE',  ( -0.000000000000000000, -0.000000000000000000, 1.000000000000000000 ) ) ;
#1094 = LINE ( 'NONE', #3399, #2408 ) ;
#1095 = EDGE_CURVE ( 'NONE', #1430, #3154, #1291, .T. ) ;
#1096 = ORIENTED_EDGE ( 'NONE', *, *, #3247, .T. ) ;
#1097 = LINE ( 'NONE', #20, #2884 ) ;
#1098 = PLANE ( 'NONE',  #1638 ) ;
#1099 = ORIENTED_EDGE ( 'NONE', *, *, #1951, .F. ) ;
#1100 = CARTESIAN_POINT ( 'NONE',  ( 19.30673457630784995, 12.49999999999993783, -12.00000000000000000 ) ) ;
#1101 = MECHANICAL_DESIGN_GEOMETRIC_PRESENTATION_REPRESENTATION (  '', ( #478 ), #1495 ) ;
#1102 = DIRECTION ( 'NONE',  ( -1.000000000000000000, -0.000000000000000000, -0.000000000000000000 ) ) ;
#1103 = CARTESIAN_POINT ( 'NONE',  ( 2.500000000000000000, -2.357898499370432610, 3.252606517456513302E-15 ) ) ;
#1104 = FACE_OUTER_BOUND ( 'NONE', #1169, .T. ) ;
#1105 = ORIENTED_EDGE ( 'NONE', *, *, #450, .T. ) ;
#1106 = AXIS2_PLACEMENT_3D ( 'NONE', #2671, #1480, #4508 ) ;
#1107 = EDGE_CURVE ( 'NONE', #3361, #4685, #866, .T. ) ;
#1108 = FACE_OUTER_BOUND ( 'NONE', #2742, .T. ) ;
#1109 = CARTESIAN_POINT ( 'NONE',  ( 19.00000000000018474, 15.99999999999971934, -26.00000000000004263 ) ) ;
#1110 = LINE ( 'NONE', #4845, #1369 ) ;
#1111 = DIRECTION ( 'NONE',  ( -0.000000000000000000, -0.000000000000000000, -1.000000000000000000 ) ) ;
#1112 = CARTESIAN_POINT ( 'NONE',  ( -19.30673457630785350, -12.49999999999993250, -12.00000000000000000 ) ) ;
#1113 = ORIENTED_EDGE ( 'NONE', *, *, #1249, .T. ) ;
#1114 = CARTESIAN_POINT ( 'NONE',  ( 0.000000000000000000, 0.000000000000000000, -20.00000000000000000 ) ) ;
#1115 = DIRECTION ( 'NONE',  ( 1.000000000000000000, 0.000000000000000000, 0.000000000000000000 ) ) ;
#1116 = EDGE_CURVE ( 'NONE', #1461, #1923, #2568, .T. ) ;
#1117 = DIRECTION ( 'NONE',  ( 0.000000000000000000, -1.000000000000000000, 1.467581828789149729E-15 ) ) ;
#1118 = AXIS2_PLACEMENT_3D ( 'NONE', #3796, #3850, #2357 ) ;
#1119 = ORIENTED_EDGE ( 'NONE', *, *, #4580, .F. ) ;
#1120 = EDGE_CURVE ( 'NONE', #1203, #991, #1604, .T. ) ;
#1121 = EDGE_CURVE ( 'NONE', #4243, #3154, #2398, .T. ) ;
#1122 = DIRECTION ( 'NONE',  ( -0.000000000000000000, -0.000000000000000000, 1.000000000000000000 ) ) ;
#1123 = DIRECTION ( 'NONE',  ( -0.000000000000000000, 0.000000000000000000, 1.000000000000000000 ) ) ;
#1124 = PRODUCT_DEFINITION_SHAPE ( 'NONE', 'NONE',  #4964 ) ;
#1125 = ORIENTED_EDGE ( 'NONE', *, *, #3211, .T. ) ;
#1126 = CIRCLE ( 'NONE', #4884, 6.999999999999999112 ) ;
#1127 = CONICAL_SURFACE ( 'NONE', #3765, 2.099999999999997868, 1.029744258676653423 ) ;
#1128 = CYLINDRICAL_SURFACE ( 'NONE', #1851, 2.000000000000000888 ) ;
#1129 = VECTOR ( 'NONE', #2895, 1000.000000000000114 ) ;
#1130 = DIRECTION ( 'NONE',  ( 1.000000000000000000, 0.000000000000000000, 0.000000000000000000 ) ) ;
#1131 = CARTESIAN_POINT ( 'NONE',  ( 0.000000000000000000, 0.000000000000000000, 4.000000000000000000 ) ) ;
#1132 = DIRECTION ( 'NONE',  ( -0.5000000000000051070, 0.000000000000000000, 0.8660254037844355990 ) ) ;
#1133 = EDGE_LOOP ( 'NONE', ( #1119, #2771, #3567, #1730 ) ) ;
#1134 = CIRCLE ( 'NONE', #2576, 23.00000000000000711 ) ;
#1135 = DIRECTION ( 'NONE',  ( 0.000000000000000000, -1.287488025362403787E-15, -1.000000000000000000 ) ) ;
#1136 = PRESENTATION_STYLE_ASSIGNMENT (( #3806 ) ) ;
#1137 = CARTESIAN_POINT ( 'NONE',  ( 0.1999999999999987899, 0.000000000000000000, 0.000000000000000000 ) ) ;
#1138 = CARTESIAN_POINT ( 'NONE',  ( -8.500000000000000000, -21.37171027316251681, 12.00000000000000000 ) ) ;
#1139 = VECTOR ( 'NONE', #2847, 1000.000000000000000 ) ;
#1140 = CARTESIAN_POINT ( 'NONE',  ( 2.000000000000000000, -0.8865213383406690406, 1.535500000000000975 ) ) ;
#1141 = STYLED_ITEM ( 'NONE', ( #908 ), #1999 ) ;
#1142 = ORIENTED_EDGE ( 'NONE', *, *, #4505, .F. ) ;
#1143 = VECTOR ( 'NONE', #4180, 1000.000000000000000 ) ;
#1144 = AXIS2_PLACEMENT_3D ( 'NONE', #891, #2352, #3950 ) ;
#1145 = FACE_OUTER_BOUND ( 'NONE', #2865, .T. ) ;
#1146 = CARTESIAN_POINT ( 'NONE',  ( 0.000000000000000000, 0.000000000000000000, 0.000000000000000000 ) ) ;
#1147 = CARTESIAN_POINT ( 'NONE',  ( 15.00000000000000000, 16.00000000000000000, -26.00000000000000355 ) ) ;
#1148 = FACE_OUTER_BOUND ( 'NONE', #3721, .T. ) ;
#1149 = AXIS2_PLACEMENT_3D ( 'NONE', #2228, #1470, #1993 ) ;
#1150 = VERTEX_POINT ( 'NONE', #3180 ) ;
#1151 = CYLINDRICAL_SURFACE ( 'NONE', #3829, 25.00000000000000000 ) ;
#1152 = FILL_AREA_STYLE_COLOUR ( '', #674 ) ;
#1153 = ORIENTED_EDGE ( 'NONE', *, *, #1637, .F. ) ;
#1154 = EDGE_CURVE ( 'NONE', #675, #2827, #2893, .T. ) ;
#1155 = EDGE_CURVE ( 'NONE', #1504, #1323, #526, .T. ) ;
#1156 = ORIENTED_EDGE ( 'NONE', *, *, #3546, .T. ) ;
#1157 = AXIS2_PLACEMENT_3D ( 'NONE', #2564, #333, #4084 ) ;
#1158 = CARTESIAN_POINT ( 'NONE',  ( 22.76902711785762534, -10.32479573876449486, -24.01193718893786411 ) ) ;
#1159 = DIRECTION ( 'NONE',  ( 0.000000000000000000, 0.000000000000000000, -1.000000000000000000 ) ) ;
#1160 = CARTESIAN_POINT ( 'NONE',  ( 2.302289838212012812E-14, -16.00000000000000000, -26.00000000000000355 ) ) ;
#1161 = DIRECTION ( 'NONE',  ( -0.000000000000000000, -0.000000000000000000, 1.000000000000000000 ) ) ;
#1162 = EDGE_CURVE ( 'NONE', #4131, #3536, #1946, .T. ) ;
#1163 = EDGE_LOOP ( 'NONE', ( #929, #3191, #2786, #3592, #1633, #1962 ) ) ;
#1164 = DIRECTION ( 'NONE',  ( 1.000000000000000000, -0.000000000000000000, -0.000000000000000000 ) ) ;
#1165 = DIRECTION ( 'NONE',  ( -0.02118582507427605247, -0.9997755552202315377, -9.765537692533071851E-17 ) ) ;
#1166 = DIRECTION ( 'NONE',  ( 0.000000000000000000, 0.000000000000000000, 1.000000000000000000 ) ) ;
#1167 = DIRECTION ( 'NONE',  ( -1.000000000000000000, 0.000000000000000000, -0.000000000000000000 ) ) ;
#1168 = CARTESIAN_POINT ( 'NONE',  ( 22.30769810302473388, 11.28612666381332730, -31.98709346889334881 ) ) ;
#1169 = EDGE_LOOP ( 'NONE', ( #2876, #3862, #4101, #2317 ) ) ;
#1170 = EDGE_LOOP ( 'NONE', ( #1550, #3395, #4871, #3982 ) ) ;
#1171 = CARTESIAN_POINT ( 'NONE',  ( 0.000000000000000000, 0.000000000000000000, -4.000000000000000000 ) ) ;
#1172 = DIRECTION ( 'NONE',  ( -0.000000000000000000, 0.8660254037844390407, 0.4999999999999993339 ) ) ;
#1173 = PLANE ( 'NONE',  #187 ) ;
#1174 = ORIENTED_EDGE ( 'NONE', *, *, #4886, .F. ) ;
#1175 = PLANE ( 'NONE',  #3916 ) ;
#1176 = EDGE_CURVE ( 'NONE', #4766, #1283, #3527, .T. ) ;
#1177 = CARTESIAN_POINT ( 'NONE',  ( 0.000000000000000000, 1.773042676681340968, -2.276824562219559311E-15 ) ) ;
#1178 = ADVANCED_FACE ( 'NONE', ( #2145 ), #4808, .F. ) ;
#1179 = VERTEX_POINT ( 'NONE', #1664 ) ;
#1180 = ORIENTED_EDGE ( 'NONE', *, *, #2385, .F. ) ;
#1181 = PRODUCT_DEFINITION ( 'UNKNOWN', '', #4711, #3035 ) ;
#1182 = EDGE_CURVE ( 'NONE', #4937, #2834, #3660, .T. ) ;
#1183 = CYLINDRICAL_SURFACE ( 'NONE', #4656, 2.099999999999994316 ) ;
#1184 = CARTESIAN_POINT ( 'NONE',  ( -23.00000000000000711, 0.000000000000000000, 4.000000000000000000 ) ) ;
#1185 = LINE ( 'NONE', #1931, #738 ) ;
#1186 = ORIENTED_EDGE ( 'NONE', *, *, #2562, .T. ) ;
#1187 = EDGE_CURVE ( 'NONE', #4462, #1525, #961, .T. ) ;
#1188 = COLOUR_RGB ( '', 0.09019608, 0.27058824, 0.51372549) ;
#1189 = DIRECTION ( 'NONE',  ( -0.02118582507427605247, -0.9997755552202315377, -9.765537692533071851E-17 ) ) ;
#1190 = DIRECTION ( 'NONE',  ( -1.000000000000000000, -0.000000000000000000, -0.000000000000000000 ) ) ;
#1191 = DIRECTION ( 'NONE',  ( 0.000000000000000000, 0.000000000000000000, -1.000000000000000000 ) ) ;
#1192 = CARTESIAN_POINT ( 'NONE',  ( 22.21646894734064759, -11.46466559648295558, -20.06384827235568835 ) ) ;
#1193 = ORIENTED_EDGE ( 'NONE', *, *, #2053, .T. ) ;
#1194 = ORIENTED_EDGE ( 'NONE', *, *, #271, .T. ) ;
#1195 = DIRECTION ( 'NONE',  ( -1.000000000000000000, -0.000000000000000000, -0.000000000000000000 ) ) ;
#1196 = LINE ( 'NONE', #3519, #1378 ) ;
#1197 = DIRECTION ( 'NONE',  ( 0.000000000000000000, 0.000000000000000000, -1.000000000000000000 ) ) ;
#1198 = ORIENTED_EDGE ( 'NONE', *, *, #2102, .T. ) ;
#1199 = FACE_OUTER_BOUND ( 'NONE', #77, .T. ) ;
#1200 = DIRECTION ( 'NONE',  ( -1.000000000000000000, 0.000000000000000000, 0.000000000000000000 ) ) ;
#1201 = AXIS2_PLACEMENT_3D ( 'NONE', #2326, #3108, #3403 ) ;
#1202 = VERTEX_POINT ( 'NONE', #3638 ) ;
#1203 = VERTEX_POINT ( 'NONE', #4060 ) ;
#1204 = EDGE_CURVE ( 'NONE', #1722, #1390, #2521, .T. ) ;
#1205 = AXIS2_PLACEMENT_3D ( 'NONE', #2976, #4465, #4097 ) ;
#1206 = CARTESIAN_POINT ( 'NONE',  ( 22.18526740102420547, -11.52862861652370441, -30.01896866400023356 ) ) ;
#1207 = DIRECTION ( 'NONE',  ( 1.000000000000000000, 0.000000000000000000, 0.000000000000000000 ) ) ;
#1208 = CARTESIAN_POINT ( 'NONE',  ( 2.500000000000000000, 0.000000000000000000, 0.000000000000000000 ) ) ;
#1209 = VERTEX_POINT ( 'NONE', #4775 ) ;
#1210 = ORIENTED_EDGE ( 'NONE', *, *, #4882, .T. ) ;
#1211 = PRODUCT_DEFINITION_SHAPE ( 'NONE', 'NONE',  #2072 ) ;
#1212 = VECTOR ( 'NONE', #4165, 1000.000000000000000 ) ;
#1213 = PLANE ( 'NONE',  #1216 ) ;
#1214 = DIRECTION ( 'NONE',  ( 0.000000000000000000, 0.000000000000000000, 1.000000000000000000 ) ) ;
#1215 = DIRECTION ( 'NONE',  ( -0.000000000000000000, -0.000000000000000000, 1.000000000000000000 ) ) ;
#1216 = AXIS2_PLACEMENT_3D ( 'NONE', #2289, #805, #2369 ) ;
#1217 = EDGE_CURVE ( 'NONE', #1044, #2709, #4037, .T. ) ;
#1218 = ORIENTED_EDGE ( 'NONE', *, *, #1217, .T. ) ;
#1219 =( NAMED_UNIT ( * ) SI_UNIT ( $, .STERADIAN. ) SOLID_ANGLE_UNIT ( ) );
#1220 = AXIS2_PLACEMENT_3D ( 'NONE', #3313, #2212, #4477 ) ;
#1221 = CARTESIAN_POINT ( 'NONE',  ( 0.000000000000000000, 25.00000000000000000, -32.00000000000000000 ) ) ;
#1222 = VECTOR ( 'NONE', #4199, 1000.000000000000000 ) ;
#1223 = FACE_OUTER_BOUND ( 'NONE', #4578, .T. ) ;
#1224 = LINE ( 'NONE', #3520, #266 ) ;
#1225 = EDGE_LOOP ( 'NONE', ( #3596, #4059, #4019, #985 ) ) ;
#1226 = AXIS2_PLACEMENT_3D ( 'NONE', #1449, #402, #1496 ) ;
#1227 = AXIS2_PLACEMENT_3D ( 'NONE', #2025, #867, #476 ) ;
#1228 = FACE_OUTER_BOUND ( 'NONE', #3061, .T. ) ;
#1229 = LINE ( 'NONE', #67, #4473 ) ;
#1230 = AXIS2_PLACEMENT_3D ( 'NONE', #88, #1590, #4909 ) ;
#1231 = ORIENTED_EDGE ( 'NONE', *, *, #1820, .F. ) ;
#1232 = ORIENTED_EDGE ( 'NONE', *, *, #1612, .T. ) ;
#1233 = AXIS2_PLACEMENT_3D ( 'NONE', #4436, #1013, #634 ) ;
#1234 = CARTESIAN_POINT ( 'NONE',  ( 22.66008913276283110, -10.56067522606771547, -23.45956100436263725 ) ) ;
#1235 = FILL_AREA_STYLE ('',( #465 ) ) ;
#1236 = DIRECTION ( 'NONE',  ( -1.000000000000000000, 0.000000000000000000, 0.000000000000000000 ) ) ;
#1237 = ORIENTED_EDGE ( 'NONE', *, *, #4276, .F. ) ;
#1238 = EDGE_LOOP ( 'NONE', ( #152, #2360, #308, #499 ) ) ;
#1239 = APPLICATION_PROTOCOL_DEFINITION ( 'draft international standard', 'automotive_design', 1998, #1377 ) ;
#1240 = EDGE_CURVE ( 'NONE', #3948, #392, #3931, .T. ) ;
#1241 = DIRECTION ( 'NONE',  ( 1.000000000000000000, -0.000000000000000000, -0.000000000000000000 ) ) ;
#1242 = EDGE_CURVE ( 'NONE', #2366, #165, #942, .T. ) ;
#1243 = CARTESIAN_POINT ( 'NONE',  ( 0.000000000000000000, -25.00000000000000000, -20.00000000000000000 ) ) ;
#1244 = LINE ( 'NONE', #2091, #822 ) ;
#1245 = AXIS2_PLACEMENT_3D ( 'NONE', #3331, #4858, #1047 ) ;
#1246 = ORIENTED_EDGE ( 'NONE', *, *, #166, .T. ) ;
#1247 = ORIENTED_EDGE ( 'NONE', *, *, #1242, .T. ) ;
#1248 = CARTESIAN_POINT ( 'NONE',  ( 6.999999999999999112, 0.000000000000000000, -32.00000000000000000 ) ) ;
#1249 = EDGE_CURVE ( 'NONE', #2708, #3361, #4014, .T. ) ;
#1250 = DIRECTION ( 'NONE',  ( 0.000000000000000000, 0.000000000000000000, -1.000000000000000000 ) ) ;
#1251 = LINE ( 'NONE', #2608, #4905 ) ;
#1252 = ORIENTED_EDGE ( 'NONE', *, *, #8, .T. ) ;
#1253 = FACE_OUTER_BOUND ( 'NONE', #3079, .T. ) ;
#1254 = EDGE_CURVE ( 'NONE', #340, #4850, #641, .T. ) ;
#1255 = CARTESIAN_POINT ( 'NONE',  ( 0.000000000000000000, 0.000000000000000000, 4.000000000000000000 ) ) ;
#1256 = ORIENTED_EDGE ( 'NONE', *, *, #2102, .F. ) ;
#1257 = PRODUCT_DEFINITION_SHAPE ( 'NONE', 'NONE',  #4971 ) ;
#1258 = EDGE_LOOP ( 'NONE', ( #1815, #3183, #2999, #3488 ) ) ;
#1259 = DIRECTION ( 'NONE',  ( 0.000000000000000000, 0.000000000000000000, 1.000000000000000000 ) ) ;
#1260 = DIRECTION ( 'NONE',  ( -0.000000000000000000, -0.000000000000000000, -1.000000000000000000 ) ) ;
#1261 = ORIENTED_EDGE ( 'NONE', *, *, #3181, .T. ) ;
#1262 = VERTEX_POINT ( 'NONE', #2170 ) ;
#1263 = FACE_OUTER_BOUND ( 'NONE', #1825, .T. ) ;
#1264 = DIRECTION ( 'NONE',  ( 4.073394895316987600E-15, -1.000000000000000000, 0.000000000000000000 ) ) ;
#1265 = CARTESIAN_POINT ( 'NONE',  ( 2.000000000000000000, 0.8865213383406717051, 1.535499999999998533 ) ) ;
#1266 = EDGE_LOOP ( 'NONE', ( #3202, #3863, #2347, #3636 ) ) ;
#1267 = STYLED_ITEM ( 'NONE', ( #1990 ), #755 ) ;
#1268 = ORIENTED_EDGE ( 'NONE', *, *, #3417, .T. ) ;
#1269 =( NAMED_UNIT ( * ) PLANE_ANGLE_UNIT ( ) SI_UNIT ( $, .RADIAN. ) );
#1270 = DIRECTION ( 'NONE',  ( 0.000000000000000000, -1.000000000000000000, 0.000000000000000000 ) ) ;
#1271 = DIRECTION ( 'NONE',  ( 0.000000000000000000, 0.000000000000000000, 1.000000000000000000 ) ) ;
#1272 = ORIENTED_EDGE ( 'NONE', *, *, #233, .F. ) ;
#1273 = EDGE_CURVE ( 'NONE', #1595, #4266, #1357, .T. ) ;
#1274 = CYLINDRICAL_SURFACE ( 'NONE', #4467, 25.00000000000000000 ) ;
#1275 = DIRECTION ( 'NONE',  ( 0.000000000000000000, 0.000000000000000000, 1.000000000000000000 ) ) ;
#1276 = ORIENTED_EDGE ( 'NONE', *, *, #4303, .T. ) ;
#1277 = ORIENTED_EDGE ( 'NONE', *, *, #547, .T. ) ;
#1278 = EDGE_CURVE ( 'NONE', #2641, #2827, #247, .T. ) ;
#1279 = EDGE_CURVE ( 'NONE', #941, #467, #3055, .T. ) ;
#1280 = CIRCLE ( 'NONE', #3357, 4.000000000000000000 ) ;
#1281 = LINE ( 'NONE', #4330, #3316 ) ;
#1282 = DIRECTION ( 'NONE',  ( 1.000000000000000000, 0.000000000000000000, 0.000000000000000000 ) ) ;
#1283 = VERTEX_POINT ( 'NONE', #3291 ) ;
#1284 = AXIS2_PLACEMENT_3D ( 'NONE', #4119, #4902, #2527 ) ;
#1285 = ORIENTED_EDGE ( 'NONE', *, *, #4911, .F. ) ;
#1286 = DIRECTION ( 'NONE',  ( -1.000000000000000000, 0.000000000000000000, 0.000000000000000000 ) ) ;
#1287 = CIRCLE ( 'NONE', #4074, 2.500000000000001332 ) ;
#1288 = FACE_OUTER_BOUND ( 'NONE', #2721, .T. ) ;
#1289 = FACE_OUTER_BOUND ( 'NONE', #4132, .T. ) ;
#1290 = ORIENTED_EDGE ( 'NONE', *, *, #4955, .T. ) ;
#1291 = CIRCLE ( 'NONE', #169, 23.00000000000000711 ) ;
#1292 = ORIENTED_EDGE ( 'NONE', *, *, #2610, .T. ) ;
#1293 = CARTESIAN_POINT ( 'NONE',  ( -14.00000000000006395, 16.00000000000000000, -26.00000000000000355 ) ) ;
#1294 = DIRECTION ( 'NONE',  ( -1.000000000000000000, -0.000000000000000000, -0.000000000000000000 ) ) ;
#1295 = VECTOR ( 'NONE', #3176, 1000.000000000000000 ) ;
#1296 = LINE ( 'NONE', #3591, #915 ) ;
#1297 = CIRCLE ( 'NONE', #3372, 25.00000000000000000 ) ;
#1298 = ORIENTED_EDGE ( 'NONE', *, *, #2437, .T. ) ;
#1299 = AXIS2_PLACEMENT_3D ( 'NONE', #3607, #186, #4006 ) ;
#1300 = AXIS2_PLACEMENT_3D ( 'NONE', #229, #4403, #603 ) ;
#1301 = CARTESIAN_POINT ( 'NONE',  ( 0.000000000000000000, 0.000000000000000000, 12.00000000000000000 ) ) ;
#1302 = PLANE ( 'NONE',  #3212 ) ;
#1303 = CIRCLE ( 'NONE', #2022, 2.649999999999995914 ) ;
#1304 = AXIS2_PLACEMENT_3D ( 'NONE', #4109, #3708, #4864 ) ;
#1305 = CIRCLE ( 'NONE', #1144, 25.00000000000000000 ) ;
#1306 = EDGE_LOOP ( 'NONE', ( #4774, #1285, #3515, #1292 ) ) ;
#1307 = VECTOR ( 'NONE', #2791, 1000.000000000000000 ) ;
#1308 = CARTESIAN_POINT ( 'NONE',  ( 2.500000000000000000, 0.000000000000000000, 0.000000000000000000 ) ) ;
#1309 = CIRCLE ( 'NONE', #3684, 0.2500000000000002220 ) ;
#1310 =( NAMED_UNIT ( * ) PLANE_ANGLE_UNIT ( ) SI_UNIT ( $, .RADIAN. ) );
#1311 = CARTESIAN_POINT ( 'NONE',  ( 0.000000000000000000, 0.000000000000000000, -20.00000000000000000 ) ) ;
#1312 = EDGE_LOOP ( 'NONE', ( #3317, #1232, #2731, #3928, #2819, #959, #2054, #4784, #3946, #4335, #3757, #4091 ) ) ;
#1313 = VERTEX_POINT ( 'NONE', #1340 ) ;
#1314 = AXIS2_PLACEMENT_3D ( 'NONE', #1789, #4511, #4090 ) ;
#1315 = CARTESIAN_POINT ( 'NONE',  ( -2.042664716792774803E-14, 16.00000000000000000, -26.00000000000000355 ) ) ;
#1316 = EDGE_CURVE ( 'NONE', #2020, #1912, #4082, .T. ) ;
#1317 = CARTESIAN_POINT ( 'NONE',  ( -9.000000000000001776, 3.903127820947817540E-15, -20.00000000000000000 ) ) ;
#1318 = CARTESIAN_POINT ( 'NONE',  ( 2.000000000000000000, 1.773042676681340968, -2.276824562219559311E-15 ) ) ;
#1319 = VERTEX_POINT ( 'NONE', #3970 ) ;
#1320 = VERTEX_POINT ( 'NONE', #564 ) ;
#1321 = DIRECTION ( 'NONE',  ( 1.000000000000000000, -0.000000000000000000, -0.000000000000000000 ) ) ;
#1322 = FACE_OUTER_BOUND ( 'NONE', #2719, .T. ) ;
#1323 = VERTEX_POINT ( 'NONE', #4434 ) ;
#1324 = CARTESIAN_POINT ( 'NONE',  ( 2.000000000000000000, 0.8865213383406685965, -1.535500000000000753 ) ) ;
#1325 = DIRECTION ( 'NONE',  ( -0.7071067811865487940, 8.659560562354948882E-17, 0.7071067811865463515 ) ) ;
#1326 = SHAPE_REPRESENTATION ( 'socket head cap screw_iso_ISO 4762 M4 x 20 - 20N', ( #1918 ), #2148 ) ;
#1327 = VERTEX_POINT ( 'NONE', #1011 ) ;
#1328 = UNCERTAINTY_MEASURE_WITH_UNIT (LENGTH_MEASURE( 1.000000000000000082E-05 ), #443, 'distance_accuracy_value', 'NONE');
#1329 = ADVANCED_FACE ( 'NONE', ( #2541 ), #545, .T. ) ;
#1330 = LINE ( 'NONE', #249, #3792 ) ;
#1331 = SHAPE_DEFINITION_REPRESENTATION ( #1603, #2032 ) ;
#1332 = ORIENTED_EDGE ( 'NONE', *, *, #2562, .F. ) ;
#1333 = EDGE_CURVE ( 'NONE', #4568, #484, #2018, .T. ) ;
#1334 = CARTESIAN_POINT ( 'NONE',  ( 0.000000000000000000, 5.051668046482832750E-16, -4.000000000000000000 ) ) ;
#1335 = DIRECTION ( 'NONE',  ( 1.000000000000000000, -3.357200482488897685E-15, 0.000000000000000000 ) ) ;
#1336 = FACE_OUTER_BOUND ( 'NONE', #4607, .T. ) ;
#1337 = ORIENTED_EDGE ( 'NONE', *, *, #746, .T. ) ;
#1338 = ADVANCED_FACE ( 'NONE', ( #2859 ), #3251, .T. ) ;
#1339 = VERTEX_POINT ( 'NONE', #1063 ) ;
#1340 = CARTESIAN_POINT ( 'NONE',  ( -21.37171027316253102, -8.499999999999925393, -12.00000000000000000 ) ) ;
#1341 = CARTESIAN_POINT ( 'NONE',  ( -13.99999999999993250, -16.00000000000000000, -26.00000000000000355 ) ) ;
#1342 = CARTESIAN_POINT ( 'NONE',  ( 5.200000000000002842, 0.000000000000000000, 0.000000000000000000 ) ) ;
#1343 = VERTEX_POINT ( 'NONE', #4509 ) ;
#1344 = DIRECTION ( 'NONE',  ( -1.000000000000000000, 0.000000000000000000, 0.000000000000000000 ) ) ;
#1345 = DIRECTION ( 'NONE',  ( 0.000000000000000000, 0.000000000000000000, -1.000000000000000000 ) ) ;
#1346 = EDGE_LOOP ( 'NONE', ( #2389, #3226, #794 ) ) ;
#1347 = DIRECTION ( 'NONE',  ( -1.000000000000000000, 0.000000000000000000, 0.000000000000000000 ) ) ;
#1348 = ORIENTED_EDGE ( 'NONE', *, *, #78, .T. ) ;
#1349 = DIRECTION ( 'NONE',  ( -1.000000000000000000, -0.000000000000000000, -0.000000000000000000 ) ) ;
#1350 = FACE_OUTER_BOUND ( 'NONE', #1431, .T. ) ;
#1351 = VECTOR ( 'NONE', #2106, 1000.000000000000000 ) ;
#1352 = FACE_OUTER_BOUND ( 'NONE', #3474, .T. ) ;
#1353 = ADVANCED_FACE ( 'NONE', ( #3340 ), #2737, .T. ) ;
#1354 = EDGE_LOOP ( 'NONE', ( #4517, #3277, #3266, #262 ) ) ;
#1355 = ORIENTED_EDGE ( 'NONE', *, *, #3411, .T. ) ;
#1356 =( NAMED_UNIT ( * ) PLANE_ANGLE_UNIT ( ) SI_UNIT ( $, .RADIAN. ) );
#1357 = LINE ( 'NONE', #4388, #2414 ) ;
#1358 = CARTESIAN_POINT ( 'NONE',  ( -10.00000000000002132, 16.00000000000000000, -28.10000000000000142 ) ) ;
#1359 = DIRECTION ( 'NONE',  ( 1.000000000000000000, 0.000000000000000000, 0.000000000000000000 ) ) ;
#1360 = EDGE_CURVE ( 'NONE', #3389, #216, #2941, .T. ) ;
#1361 = EDGE_CURVE ( 'NONE', #3396, #3754, #4924, .T. ) ;
#1362 = AXIS2_PLACEMENT_3D ( 'NONE', #1897, #3377, #2606 ) ;
#1363 = ORIENTED_EDGE ( 'NONE', *, *, #1576, .T. ) ;
#1364 = CARTESIAN_POINT ( 'NONE',  ( 25.00000000000000000, 0.000000000000000000, -20.00000000000000000 ) ) ;
#1365 = CARTESIAN_POINT ( 'NONE',  ( -31.74999999999995737, 2.449293598294707893E-16, -2.000000000000000888 ) ) ;
#1366 = EDGE_CURVE ( 'NONE', #4359, #318, #4531, .T. ) ;
#1367 = ORIENTED_EDGE ( 'NONE', *, *, #4600, .F. ) ;
#1368 = CIRCLE ( 'NONE', #2824, 6.999999999999999112 ) ;
#1369 = VECTOR ( 'NONE', #1501, 1000.000000000000000 ) ;
#1370 = LINE ( 'NONE', #672, #4067 ) ;
#1371 = CARTESIAN_POINT ( 'NONE',  ( 5.000000000000004441, 5.204748896376250699E-16, -4.250000000000000000 ) ) ;
#1372 = PLANE ( 'NONE',  #4488 ) ;
#1373 = AXIS2_PLACEMENT_3D ( 'NONE', #4363, #2088, #955 ) ;
#1374 = PRODUCT ( 'BR-550', 'BR-550', '', ( #4260 ) ) ;
#1375 = ORIENTED_EDGE ( 'NONE', *, *, #271, .F. ) ;
#1376 = AXIS2_PLACEMENT_3D ( 'NONE', #3753, #4202, #3409 ) ;
#1377 = APPLICATION_CONTEXT ( 'automotive_design' ) ;
#1378 = VECTOR ( 'NONE', #3497, 1000.000000000000114 ) ;
#1379 = CARTESIAN_POINT ( 'NONE',  ( 0.000000000000000000, 0.000000000000000000, -32.00000000000000000 ) ) ;
#1380 = DIRECTION ( 'NONE',  ( -1.000000000000000000, -0.000000000000000000, -0.000000000000000000 ) ) ;
#1381 = STYLED_ITEM ( 'NONE', ( #2956 ), #3609 ) ;
#1382 = CARTESIAN_POINT ( 'NONE',  ( 2.000000000000000000, 2.253471898105738645E-15, 1.535499999999999865 ) ) ;
#1383 = ORIENTED_EDGE ( 'NONE', *, *, #2555, .F. ) ;
#1384 = DIRECTION ( 'NONE',  ( 1.000000000000000000, 0.000000000000000000, 0.000000000000000000 ) ) ;
#1385 = EDGE_CURVE ( 'NONE', #451, #3363, #1110, .T. ) ;
#1386 =( LENGTH_UNIT ( ) NAMED_UNIT ( * ) SI_UNIT ( .MILLI., .METRE. ) );
#1387 = DIRECTION ( 'NONE',  ( 0.000000000000000000, 0.000000000000000000, -1.000000000000000000 ) ) ;
#1388 = LINE ( 'NONE', #1358, #4480 ) ;
#1389 = DIRECTION ( 'NONE',  ( 1.000000000000000000, -0.000000000000000000, -0.000000000000000000 ) ) ;
#1390 = VERTEX_POINT ( 'NONE', #2638 ) ;
#1391 = ORIENTED_EDGE ( 'NONE', *, *, #3477, .T. ) ;
#1392 =( LENGTH_UNIT ( ) NAMED_UNIT ( * ) SI_UNIT ( .MILLI., .METRE. ) );
#1393 = AXIS2_PLACEMENT_3D ( 'NONE', #629, #3391, #4433 ) ;
#1394 = LINE ( 'NONE', #4757, #2168 ) ;
#1395 = VERTEX_POINT ( 'NONE', #1458 ) ;
#1396 = EDGE_CURVE ( 'NONE', #586, #3657, #2656, .T. ) ;
#1397 = CARTESIAN_POINT ( 'NONE',  ( 0.000000000000000000, -1.773042676681340968, 2.059984127722458425E-15 ) ) ;
#1398 = DIRECTION ( 'NONE',  ( 3.357200482488897290E-15, 1.000000000000000000, 0.000000000000000000 ) ) ;
#1399 = DIRECTION ( 'NONE',  ( -0.000000000000000000, -0.000000000000000000, 1.000000000000000000 ) ) ;
#1400 = VERTEX_POINT ( 'NONE', #4134 ) ;
#1401 = CARTESIAN_POINT ( 'NONE',  ( -9.999999999999975131, -16.00000000000000000, -26.00000000000000355 ) ) ;
#1402 = CARTESIAN_POINT ( 'NONE',  ( -3.041771206386918902E-14, -8.500000000000001776, -12.00000000000000000 ) ) ;
#1403 = CARTESIAN_POINT ( 'NONE',  ( 0.000000000000000000, 0.000000000000000000, 4.000000000000000000 ) ) ;
#1404 = EDGE_LOOP ( 'NONE', ( #4681, #3073, #3892 ) ) ;
#1405 = CARTESIAN_POINT ( 'NONE',  ( 0.000000000000000000, 0.000000000000000000, -12.00000000000000000 ) ) ;
#1406 = DIRECTION ( 'NONE',  ( -0.000000000000000000, -0.000000000000000000, 1.000000000000000000 ) ) ;
#1407 = ADVANCED_BREP_SHAPE_REPRESENTATION ( '', ( #2009, #1918 ), #2148 ) ;
#1408 = CYLINDRICAL_SURFACE ( 'NONE', #3219, 1.000000000000000888 ) ;
#1409 = CARTESIAN_POINT ( 'NONE',  ( -4.473192950568998942E-14, -12.50000000000000178, -4.000000000000000000 ) ) ;
#1410 = ORIENTED_EDGE ( 'NONE', *, *, #4276, .T. ) ;
#1411 = ORIENTED_EDGE ( 'NONE', *, *, #547, .F. ) ;
#1412 = CYLINDRICAL_SURFACE ( 'NONE', #261, 6.999999999999999112 ) ;
#1413 = DIRECTION ( 'NONE',  ( 1.000000000000000000, 0.000000000000000000, 0.000000000000000000 ) ) ;
#1414 = LINE ( 'NONE', #4353, #2649 ) ;
#1415 = EDGE_CURVE ( 'NONE', #4685, #2641, #3296, .T. ) ;
#1416 = ORIENTED_EDGE ( 'NONE', *, *, #1982, .T. ) ;
#1417 = EDGE_CURVE ( 'NONE', #3810, #1179, #4402, .T. ) ;
#1418 = CARTESIAN_POINT ( 'NONE',  ( -2.172477277502393807E-14, 16.00000000000000000, -26.00000000000000355 ) ) ;
#1419 = DIRECTION ( 'NONE',  ( -1.000000000000000000, 0.000000000000000000, 0.000000000000000000 ) ) ;
#1420 = ADVANCED_FACE ( 'NONE', ( #2595 ), #335, .T. ) ;
#1421 = ADVANCED_FACE ( 'NONE', ( #3392 ), #658, .F. ) ;
#1422 = ORIENTED_EDGE ( 'NONE', *, *, #655, .F. ) ;
#1423 = DIRECTION ( 'NONE',  ( 0.000000000000000000, -0.4999999999999993894, 0.8660254037844389297 ) ) ;
#1424 = LINE ( 'NONE', #3707, #2981 ) ;
#1425 = ORIENTED_EDGE ( 'NONE', *, *, #3837, .T. ) ;
#1426 = PLANE ( 'NONE',  #1157 ) ;
#1427 = CARTESIAN_POINT ( 'NONE',  ( 0.2500000000000002220, 5.204748896376250699E-16, -4.250000000000000000 ) ) ;
#1428 = DIRECTION ( 'NONE',  ( 0.000000000000000000, 0.000000000000000000, -1.000000000000000000 ) ) ;
#1429 = LINE ( 'NONE', #2972, #2189 ) ;
#1430 = VERTEX_POINT ( 'NONE', #2193 ) ;
#1431 = EDGE_LOOP ( 'NONE', ( #303, #1383, #4360, #843 ) ) ;
#1432 = FACE_OUTER_BOUND ( 'NONE', #4960, .T. ) ;
#1433 = FACE_OUTER_BOUND ( 'NONE', #1585, .T. ) ;
#1434 = DIRECTION ( 'NONE',  ( -1.000000000000000000, -0.000000000000000000, -0.000000000000000000 ) ) ;
#1435 = VECTOR ( 'NONE', #792, 1000.000000000000000 ) ;
#1436 = ORIENTED_EDGE ( 'NONE', *, *, #1447, .F. ) ;
#1437 = VECTOR ( 'NONE', #3347, 1000.000000000000000 ) ;
#1438 = CARTESIAN_POINT ( 'NONE',  ( 6.497531322021036645E-14, -16.00000000000000000, -28.10000000000000142 ) ) ;
#1439 = ITEM_DEFINED_TRANSFORMATION ( 'NONE', 'NONE', #1905,  #1918 ) ;
#1440 = FACE_OUTER_BOUND ( 'NONE', #363, .T. ) ;
#1441 = VECTOR ( 'NONE', #3616, 1000.000000000000000 ) ;
#1442 = AXIS2_PLACEMENT_3D ( 'NONE', #682, #1830, #1086 ) ;
#1443 = VERTEX_POINT ( 'NONE', #3319 ) ;
#1444 = VECTOR ( 'NONE', #439, 1000.000000000000000 ) ;
#1445 = ADVANCED_FACE ( 'NONE', ( #2672 ), #1481, .F. ) ;
#1446 = CIRCLE ( 'NONE', #1300, 6.999999999999999112 ) ;
#1447 = EDGE_CURVE ( 'NONE', #2396, #654, #4893, .T. ) ;
#1448 = PLANE ( 'NONE',  #4897 ) ;
#1449 = CARTESIAN_POINT ( 'NONE',  ( 0.000000000000000000, -25.00000000000000000, -32.00000000000000000 ) ) ;
#1450 = DIRECTION ( 'NONE',  ( 1.000000000000000000, 0.000000000000000000, 0.000000000000000000 ) ) ;
#1451 = CARTESIAN_POINT ( 'NONE',  ( 2.444036937190193033E-14, 6.999999999999999112, -20.00000000000000000 ) ) ;
#1452 = AXIS2_PLACEMENT_3D ( 'NONE', #2221, #2601, #3722 ) ;
#1453 = AXIS2_PLACEMENT_3D ( 'NONE', #4587, #440, #2284 ) ;
#1454 = COLOUR_RGB ( '', 0.40784314, 0.44705882, 0.49803922) ;
#1455 = EDGE_LOOP ( 'NONE', ( #42, #2415, #3096, #2460 ) ) ;
#1456 = ORIENTED_EDGE ( 'NONE', *, *, #4572, .T. ) ;
#1457 = AXIS2_PLACEMENT_3D ( 'NONE', #1971, #2989, #3498 ) ;
#1458 = CARTESIAN_POINT ( 'NONE',  ( 2.500000000000000000, -1.178949249685218303, -2.041999999999998039 ) ) ;
#1459 = CARTESIAN_POINT ( 'NONE',  ( -4.336808689942023652E-16, 2.000000000000002220, -20.00000000000000000 ) ) ;
#1460 = FACE_OUTER_BOUND ( 'NONE', #4318, .T. ) ;
#1461 = VERTEX_POINT ( 'NONE', #1427 ) ;
#1462 = AXIS2_PLACEMENT_3D ( 'NONE', #1037, #4460, #4062 ) ;
#1463 = DIRECTION ( 'NONE',  ( -4.336808689942018722E-16, -1.000000000000000000, 0.000000000000000000 ) ) ;
#1464 = FACE_OUTER_BOUND ( 'NONE', #442, .T. ) ;
#1465 = DIRECTION ( 'NONE',  ( -0.000000000000000000, -0.000000000000000000, -1.000000000000000000 ) ) ;
#1466 = CARTESIAN_POINT ( 'NONE',  ( 25.00000000000000000, 0.000000000000000000, -32.00000000000000000 ) ) ;
#1467 = VERTEX_POINT ( 'NONE', #3787 ) ;
#1468 = CARTESIAN_POINT ( 'NONE',  ( 0.000000000000000000, 0.000000000000000000, -20.00000000000000000 ) ) ;
#1469 = DIRECTION ( 'NONE',  ( -1.000000000000000000, 0.000000000000000000, 0.000000000000000000 ) ) ;
#1470 = DIRECTION ( 'NONE',  ( 0.000000000000000000, 0.000000000000000000, 1.000000000000000000 ) ) ;
#1471 = CIRCLE ( 'NONE', #4031, 6.999999999999999112 ) ;
#1472 = ORIENTED_EDGE ( 'NONE', *, *, #4303, .F. ) ;
#1473 = LINE ( 'NONE', #326, #97 ) ;
#1474 = LINE ( 'NONE', #2993, #3071 ) ;
#1475 = FACE_OUTER_BOUND ( 'NONE', #3274, .T. ) ;
#1476 = DIRECTION ( 'NONE',  ( 0.000000000000000000, 0.000000000000000000, 1.000000000000000000 ) ) ;
#1477 = ORIENTED_EDGE ( 'NONE', *, *, #4419, .F. ) ;
#1478 = EDGE_CURVE ( 'NONE', #1067, #318, #1297, .T. ) ;
#1479 = ORIENTED_EDGE ( 'NONE', *, *, #4639, .T. ) ;
#1480 = DIRECTION ( 'NONE',  ( 0.000000000000000000, 0.000000000000000000, 1.000000000000000000 ) ) ;
#1481 = PLANE ( 'NONE',  #2574 ) ;
#1482 = CARTESIAN_POINT ( 'NONE',  ( 21.37171027316246708, -8.500000000000078160, -12.00000000000000000 ) ) ;
#1483 = DIRECTION ( 'NONE',  ( 0.000000000000000000, 0.000000000000000000, -1.000000000000000000 ) ) ;
#1484 = ADVANCED_FACE ( 'NONE', ( #2970 ), #3685, .T. ) ;
#1485 = ADVANCED_FACE ( 'NONE', ( #3413 ), #414, .F. ) ;
#1486 = ORIENTED_EDGE ( 'NONE', *, *, #4172, .F. ) ;
#1487 = DIRECTION ( 'NONE',  ( 1.000000000000000000, 0.000000000000000000, 0.000000000000000000 ) ) ;
#1488 = CARTESIAN_POINT ( 'NONE',  ( 19.30673457630776468, -12.50000000000007105, -12.00000000000000000 ) ) ;
#1489 = ORIENTED_EDGE ( 'NONE', *, *, #166, .F. ) ;
#1490 = UNCERTAINTY_MEASURE_WITH_UNIT (LENGTH_MEASURE( 1.000000000000000082E-05 ), #4932, 'distance_accuracy_value', 'NONE');
#1491 = CARTESIAN_POINT ( 'NONE',  ( 4.199999999999995737, 0.000000000000000000, 2.000000000000000888 ) ) ;
#1492 = CARTESIAN_POINT ( 'NONE',  ( 2.500000000000000000, 2.357898499370433054, -1.951563910473907981E-15 ) ) ;
#1493 = EDGE_LOOP ( 'NONE', ( #2466, #4792, #2319, #1627, #2622 ) ) ;
#1494 = CARTESIAN_POINT ( 'NONE',  ( 2.000000000000000000, 0.000000000000000000, 0.000000000000000000 ) ) ;
#1495 =( GEOMETRIC_REPRESENTATION_CONTEXT ( 3 ) GLOBAL_UNCERTAINTY_ASSIGNED_CONTEXT ( ( #2332 ) ) GLOBAL_UNIT_ASSIGNED_CONTEXT ( ( #1386, #309, #3637 ) ) REPRESENTATION_CONTEXT ( 'NONE', 'WORKASPACE' ) );
#1496 = DIRECTION ( 'NONE',  ( -2.036697447658493800E-15, 1.000000000000000000, 0.000000000000000000 ) ) ;
#1497 = CARTESIAN_POINT ( 'NONE',  ( -2.042664716792774803E-14, 16.00000000000000000, -28.09999999999999432 ) ) ;
#1498 = DIRECTION ( 'NONE',  ( 0.000000000000000000, -0.5000000000000012212, -0.8660254037844380415 ) ) ;
#1499 = ORIENTED_EDGE ( 'NONE', *, *, #299, .F. ) ;
#1500 = DIRECTION ( 'NONE',  ( 0.000000000000000000, -1.000000000000000000, 0.000000000000000000 ) ) ;
#1501 = DIRECTION ( 'NONE',  ( 1.000000000000000000, -3.357200482488897685E-15, 0.000000000000000000 ) ) ;
#1502 = DIRECTION ( 'NONE',  ( 0.000000000000000000, 0.000000000000000000, -1.000000000000000000 ) ) ;
#1503 = DIRECTION ( 'NONE',  ( -0.000000000000000000, -0.000000000000000000, 1.000000000000000000 ) ) ;
#1504 = VERTEX_POINT ( 'NONE', #2312 ) ;
#1505 = CIRCLE ( 'NONE', #1201, 22.99999999999998934 ) ;
#1506 = CARTESIAN_POINT ( 'NONE',  ( -9.000000000000001776, 3.903127820947817540E-15, -12.00000000000000000 ) ) ;
#1507 = SURFACE_STYLE_FILL_AREA ( #417 ) ;
#1508 = ADVANCED_FACE ( 'NONE', ( #3912 ), #3833, .F. ) ;
#1509 = CYLINDRICAL_SURFACE ( 'NONE', #3846, 25.00000000000000000 ) ;
#1510 = EDGE_CURVE ( 'NONE', #3209, #153, #1610, .T. ) ;
#1511 = FILL_AREA_STYLE_COLOUR ( '', #580 ) ;
#1512 = AXIS2_PLACEMENT_3D ( 'NONE', #2201, #637, #3326 ) ;
#1513 = ORIENTED_EDGE ( 'NONE', *, *, #2839, .F. ) ;
#1514 = LINE ( 'NONE', #2728, #4549 ) ;
#1515 = EDGE_CURVE ( 'NONE', #318, #4003, #1, .T. ) ;
#1516 = CIRCLE ( 'NONE', #3756, 25.00000000000000000 ) ;
#1517 = ORIENTED_EDGE ( 'NONE', *, *, #1694, .F. ) ;
#1518 = VERTEX_POINT ( 'NONE', #3121 ) ;
#1519 = VECTOR ( 'NONE', #3227, 1000.000000000000227 ) ;
#1520 = AXIS2_PLACEMENT_3D ( 'NONE', #3046, #3438, #2673 ) ;
#1521 = AXIS2_PLACEMENT_3D ( 'NONE', #32, #1241, #3099 ) ;
#1522 = DIRECTION ( 'NONE',  ( -1.000000000000000000, -3.784637517658031179E-16, -0.000000000000000000 ) ) ;
#1523 = CYLINDRICAL_SURFACE ( 'NONE', #4895, 23.00000000000000711 ) ;
#1524 = LINE ( 'NONE', #3785, #3614 ) ;
#1525 = VERTEX_POINT ( 'NONE', #2340 ) ;
#1526 = CIRCLE ( 'NONE', #3770, 2.041999999999999815 ) ;
#1527 = PRESENTATION_LAYER_ASSIGNMENT (  '', '', ( #1141 ) ) ;
#1528 = DIRECTION ( 'NONE',  ( 0.000000000000000000, 0.000000000000000000, 1.000000000000000000 ) ) ;
#1529 = DIRECTION ( 'NONE',  ( 0.02118582507427074768, 0.9997755552202315377, 1.853613717722139563E-17 ) ) ;
#1530 = CARTESIAN_POINT ( 'NONE',  ( 0.000000000000000000, 0.000000000000000000, 4.000000000000000000 ) ) ;
#1531 = DIRECTION ( 'NONE',  ( 0.000000000000000000, 0.000000000000000000, -1.000000000000000000 ) ) ;
#1532 = VECTOR ( 'NONE', #1102, 1000.000000000000000 ) ;
#1533 = VECTOR ( 'NONE', #1659, 1000.000000000000000 ) ;
#1534 = CARTESIAN_POINT ( 'NONE',  ( 22.40016391766193138, -11.10102051443364424, -20.00000000000000000 ) ) ;
#1535 = ORIENTED_EDGE ( 'NONE', *, *, #3247, .F. ) ;
#1536 = EDGE_CURVE ( 'NONE', #240, #153, #3462, .T. ) ;
#1537 = AXIS2_PLACEMENT_3D ( 'NONE', #750, #328, #1130 ) ;
#1538 = STYLED_ITEM ( 'NONE', ( #3422 ), #2058 ) ;
#1539 = EDGE_LOOP ( 'NONE', ( #3461, #1174, #3112, #4718 ) ) ;
#1540 = CARTESIAN_POINT ( 'NONE',  ( 4.199999999999995737, 0.000000000000000000, -2.200000000000001066 ) ) ;
#1541 = DIRECTION ( 'NONE',  ( -0.000000000000000000, -0.000000000000000000, 1.000000000000000000 ) ) ;
#1542 = VECTOR ( 'NONE', #291, 1000.000000000000000 ) ;
#1543 = EDGE_LOOP ( 'NONE', ( #4236, #4956, #2529, #1904, #4504, #4661 ) ) ;
#1544 = EDGE_CURVE ( 'NONE', #2456, #4849, #810, .T. ) ;
#1545 = ADVANCED_FACE ( 'NONE', ( #1263 ), #1213, .F. ) ;
#1546 = CLOSED_SHELL ( 'NONE', ( #784, #1484, #598, #1353, #1952, #3210, #4290, #2047, #2783, #3681, #3811, #4121, #4790, #1721, #2788, #904, #3985, #1890, #4026, #2935, #19, #3384, #2384, #2449, #158, #1545, #1797 ) ) ;
#1547 = VECTOR ( 'NONE', #446, 1000.000000000000227 ) ;
#1548 = DIRECTION ( 'NONE',  ( 0.000000000000000000, 0.000000000000000000, 1.000000000000000000 ) ) ;
#1549 = ORIENTED_EDGE ( 'NONE', *, *, #3297, .T. ) ;
#1550 = ORIENTED_EDGE ( 'NONE', *, *, #4235, .T. ) ;
#1551 = EDGE_CURVE ( 'NONE', #4747, #1202, #3934, .T. ) ;
#1552 = VECTOR ( 'NONE', #1733, 1000.000000000000000 ) ;
#1553 = AXIS2_PLACEMENT_3D ( 'NONE', #4048, #619, #4760 ) ;
#1554 = CARTESIAN_POINT ( 'NONE',  ( 22.47483654244695472, -10.94974330264383156, -29.24541893584931529 ) ) ;
#1555 = PLANE ( 'NONE',  #2113 ) ;
#1556 = CARTESIAN_POINT ( 'NONE',  ( 0.000000000000000000, 0.000000000000000000, 12.00000000000000000 ) ) ;
#1557 = LINE ( 'NONE', #4611, #4253 ) ;
#1558 = VERTEX_POINT ( 'NONE', #4592 ) ;
#1559 = DIRECTION ( 'NONE',  ( 6.982962677686266711E-15, 0.000000000000000000, -1.000000000000000000 ) ) ;
#1560 = DIRECTION ( 'NONE',  ( 1.000000000000000000, -0.000000000000000000, -0.000000000000000000 ) ) ;
#1561 = DIRECTION ( 'NONE',  ( 0.000000000000000000, 0.000000000000000000, -1.000000000000000000 ) ) ;
#1562 = DIRECTION ( 'NONE',  ( -1.000000000000000000, 0.000000000000000000, -0.000000000000000000 ) ) ;
#1563 = ORIENTED_EDGE ( 'NONE', *, *, #3872, .T. ) ;
#1564 = ORIENTED_EDGE ( 'NONE', *, *, #99, .T. ) ;
#1565 = CARTESIAN_POINT ( 'NONE',  ( 2.500000000000000000, 3.004629197474318851E-15, 2.042000000000000259 ) ) ;
#1566 = FACE_OUTER_BOUND ( 'NONE', #1632, .T. ) ;
#1567 = ORIENTED_EDGE ( 'NONE', *, *, #1945, .F. ) ;
#1568 = CARTESIAN_POINT ( 'NONE',  ( 2.500000000000000000, 1.178949249685218525, 2.041999999999999371 ) ) ;
#1569 = CARTESIAN_POINT ( 'NONE',  ( 0.000000000000000000, 1.178949249685213863, -2.042000000000001148 ) ) ;
#1570 = ORIENTED_EDGE ( 'NONE', *, *, #1637, .T. ) ;
#1571 = ADVANCED_FACE ( 'NONE', ( #2795 ), #1606, .T. ) ;
#1572 = ORIENTED_EDGE ( 'NONE', *, *, #4762, .T. ) ;
#1573 = CARTESIAN_POINT ( 'NONE',  ( 22.03949535914419755, -11.80087472665740478, -30.28571428571428470 ) ) ;
#1574 = EDGE_CURVE ( 'NONE', #3659, #2525, #1768, .T. ) ;
#1575 = DIRECTION ( 'NONE',  ( -0.000000000000000000, -0.000000000000000000, 1.000000000000000000 ) ) ;
#1576 = EDGE_CURVE ( 'NONE', #3989, #4766, #4262, .T. ) ;
#1577 = EDGE_CURVE ( 'NONE', #2525, #803, #3220, .T. ) ;
#1578 = DIRECTION ( 'NONE',  ( 1.000000000000000000, 2.168404344971009361E-16, 0.000000000000000000 ) ) ;
#1579 = ORIENTED_EDGE ( 'NONE', *, *, #233, .T. ) ;
#1580 = VERTEX_POINT ( 'NONE', #2392 ) ;
#1581 =( GEOMETRIC_REPRESENTATION_CONTEXT ( 3 ) GLOBAL_UNCERTAINTY_ASSIGNED_CONTEXT ( ( #393 ) ) GLOBAL_UNIT_ASSIGNED_CONTEXT ( ( #500, #1269, #2858 ) ) REPRESENTATION_CONTEXT ( 'NONE', 'WORKASPACE' ) );
#1582 = DIRECTION ( 'NONE',  ( 1.000000000000000000, -0.000000000000000000, -0.000000000000000000 ) ) ;
#1583 = CARTESIAN_POINT ( 'NONE',  ( -7.332110811570578784E-14, -6.999999999999999112, -20.00000000000000000 ) ) ;
#1584 = PLANE ( 'NONE',  #670 ) ;
#1585 = EDGE_LOOP ( 'NONE', ( #1499, #1942, #2195, #3333 ) ) ;
#1586 = ORIENTED_EDGE ( 'NONE', *, *, #2131, .T. ) ;
#1587 = PRESENTATION_STYLE_ASSIGNMENT (( #2242 ) ) ;
#1588 = DIRECTION ( 'NONE',  ( 0.000000000000000000, 0.000000000000000000, 1.000000000000000000 ) ) ;
#1589 = DIRECTION ( 'NONE',  ( 1.000000000000000000, 0.000000000000000000, 0.000000000000000000 ) ) ;
#1590 = DIRECTION ( 'NONE',  ( -1.000000000000000000, -0.000000000000000000, -0.000000000000000000 ) ) ;
#1591 = ORIENTED_EDGE ( 'NONE', *, *, #3546, .F. ) ;
#1592 = DIRECTION ( 'NONE',  ( 1.000000000000000000, -0.000000000000000000, -0.000000000000000000 ) ) ;
#1593 = AXIS2_PLACEMENT_3D ( 'NONE', #1418, #2954, #3772 ) ;
#1594 = VERTEX_POINT ( 'NONE', #470 ) ;
#1595 = VERTEX_POINT ( 'NONE', #3147 ) ;
#1596 = ADVANCED_FACE ( 'NONE', ( #3076 ), #1964, .T. ) ;
#1597 = CARTESIAN_POINT ( 'NONE',  ( 22.87614623887219523, -10.08384657499285808, -27.01992493973954623 ) ) ;
#1598 = DIRECTION ( 'NONE',  ( -1.357798298438996130E-15, 1.000000000000000000, 0.000000000000000000 ) ) ;
#1599 = CARTESIAN_POINT ( 'NONE',  ( -4.336808689942023652E-16, 2.000000000000002220, -12.00000000000000000 ) ) ;
#1600 = AXIS2_PLACEMENT_3D ( 'NONE', #3644, #947, #928 ) ;
#1601 = ORIENTED_EDGE ( 'NONE', *, *, #4523, .F. ) ;
#1602 = EDGE_CURVE ( 'NONE', #519, #4198, #4312, .T. ) ;
#1603 = PRODUCT_DEFINITION_SHAPE ( 'NONE', 'NONE',  #1181 ) ;
#1604 = CIRCLE ( 'NONE', #3762, 25.00000000000000000 ) ;
#1605 = APPLICATION_PROTOCOL_DEFINITION ( 'draft international standard', 'automotive_design', 1998, #1891 ) ;
#1606 = CYLINDRICAL_SURFACE ( 'NONE', #3849, 25.00000000000000000 ) ;
#1607 = DIRECTION ( 'NONE',  ( -0.000000000000000000, -0.000000000000000000, 1.000000000000000000 ) ) ;
#1608 = CARTESIAN_POINT ( 'NONE',  ( 22.40016391766193493, -11.10102051443364068, -32.00000000000000000 ) ) ;
#1609 = AXIS2_PLACEMENT_3D ( 'NONE', #1658, #4616, #1191 ) ;
#1610 = CIRCLE ( 'NONE', #1928, 2.099999999999997868 ) ;
#1611 = ORIENTED_EDGE ( 'NONE', *, *, #113, .T. ) ;
#1612 = EDGE_CURVE ( 'NONE', #2092, #4218, #3063, .T. ) ;
#1613 = ORIENTED_EDGE ( 'NONE', *, *, #913, .T. ) ;
#1614 = SURFACE_SIDE_STYLE ('',( #85 ) ) ;
#1615 = VECTOR ( 'NONE', #4309, 1000.000000000000000 ) ;
#1616 = DIRECTION ( 'NONE',  ( 0.7071067811865469066, 8.659560562354926695E-17, -0.7071067811865482389 ) ) ;
#1617 = AXIS2_PLACEMENT_3D ( 'NONE', #3584, #4430, #1006 ) ;
#1618 = PLANE ( 'NONE',  #2668 ) ;
#1619 = CARTESIAN_POINT ( 'NONE',  ( -6.708203932499366751, -2.000000000000003553, -32.00000000000000000 ) ) ;
#1620 = ORIENTED_EDGE ( 'NONE', *, *, #1095, .T. ) ;
#1621 = VECTOR ( 'NONE', #2537, 1000.000000000000000 ) ;
#1622 = PRESENTATION_LAYER_ASSIGNMENT (  '', '', ( #3776 ) ) ;
#1623 = DIRECTION ( 'NONE',  ( -0.000000000000000000, -0.000000000000000000, 1.000000000000000000 ) ) ;
#1624 = DIRECTION ( 'NONE',  ( -1.000000000000000000, 0.000000000000000000, 0.000000000000000000 ) ) ;
#1625 = CIRCLE ( 'NONE', #2753, 22.99999999999998934 ) ;
#1626 = ORIENTED_EDGE ( 'NONE', *, *, #2155, .F. ) ;
#1627 = ORIENTED_EDGE ( 'NONE', *, *, #2803, .T. ) ;
#1628 = DIRECTION ( 'NONE',  ( 1.000000000000000000, -0.000000000000000000, -0.000000000000000000 ) ) ;
#1629 = FILL_AREA_STYLE_COLOUR ( '', #2582 ) ;
#1630 = DIRECTION ( 'NONE',  ( 4.073394895316987600E-15, -1.000000000000000000, 0.000000000000000000 ) ) ;
#1631 = DIRECTION ( 'NONE',  ( 0.000000000000000000, 0.4999999999999990008, -0.8660254037844391517 ) ) ;
#1632 = EDGE_LOOP ( 'NONE', ( #2406, #416, #3683 ) ) ;
#1633 = ORIENTED_EDGE ( 'NONE', *, *, #2286, .T. ) ;
#1634 = CARTESIAN_POINT ( 'NONE',  ( -10.00000000000002132, 16.00000000000000000, -23.90000000000000568 ) ) ;
#1635 = CARTESIAN_POINT ( 'NONE',  ( -9.999999999999975131, -16.00000000000000000, -23.90000000000000568 ) ) ;
#1636 = DIRECTION ( 'NONE',  ( 0.000000000000000000, 0.000000000000000000, -1.000000000000000000 ) ) ;
#1637 = EDGE_CURVE ( 'NONE', #2708, #1327, #4332, .T. ) ;
#1638 = AXIS2_PLACEMENT_3D ( 'NONE', #4574, #4124, #3744 ) ;
#1639 = EDGE_LOOP ( 'NONE', ( #995, #871, #2214, #960 ) ) ;
#1640 = EDGE_LOOP ( 'NONE', ( #4522, #2809 ) ) ;
#1641 = FACE_OUTER_BOUND ( 'NONE', #68, .T. ) ;
#1642 = FACE_OUTER_BOUND ( 'NONE', #2000, .T. ) ;
#1643 = EDGE_CURVE ( 'NONE', #4802, #2990, #2695, .T. ) ;
#1644 = SHAPE_REPRESENTATION ( 'torque disk', ( #1918 ), #1039 ) ;
#1645 = EDGE_CURVE ( 'NONE', #1339, #3410, #2044, .T. ) ;
#1646 = ORIENTED_EDGE ( 'NONE', *, *, #400, .T. ) ;
#1647 = DIRECTION ( 'NONE',  ( -0.000000000000000000, -0.000000000000000000, -1.000000000000000000 ) ) ;
#1648 = DIRECTION ( 'NONE',  ( 1.000000000000000000, 0.000000000000000000, 0.000000000000000000 ) ) ;
#1649 = VERTEX_POINT ( 'NONE', #3263 ) ;
#1650 = PRODUCT_DEFINITION_SHAPE ( 'NONE', 'NONE',  #4969 ) ;
#1651 = ORIENTED_EDGE ( 'NONE', *, *, #4474, .F. ) ;
#1652 = DIRECTION ( 'NONE',  ( 0.000000000000000000, 0.000000000000000000, -1.000000000000000000 ) ) ;
#1653 = LINE ( 'NONE', #4734, #103 ) ;
#1654 = DIRECTION ( 'NONE',  ( 0.000000000000000000, 0.000000000000000000, -1.000000000000000000 ) ) ;
#1655 = ORIENTED_EDGE ( 'NONE', *, *, #3196, .T. ) ;
#1656 = ORIENTED_EDGE ( 'NONE', *, *, #3717, .T. ) ;
#1657 = PLANE ( 'NONE',  #3771 ) ;
#1658 = CARTESIAN_POINT ( 'NONE',  ( 5.200000000000002842, 0.000000000000000000, -2.700000000000001066 ) ) ;
#1659 = DIRECTION ( 'NONE',  ( -0.000000000000000000, -0.000000000000000000, 1.000000000000000000 ) ) ;
#1660 = ORIENTED_EDGE ( 'NONE', *, *, #1996, .T. ) ;
#1661 = MECHANICAL_DESIGN_GEOMETRIC_PRESENTATION_REPRESENTATION (  '', ( #4381 ), #4055 ) ;
#1662 = ADVANCED_FACE ( 'NONE', ( #3221 ), #2982, .F. ) ;
#1663 = EDGE_LOOP ( 'NONE', ( #3382, #4596, #3244, #1237 ) ) ;
#1664 = CARTESIAN_POINT ( 'NONE',  ( 25.00000000000000000, 0.000000000000000000, 2.055000000000000160 ) ) ;
#1665 = FACE_BOUND ( 'NONE', #136, .T. ) ;
#1666 = DIRECTION ( 'NONE',  ( -0.000000000000000000, 0.000000000000000000, 1.000000000000000000 ) ) ;
#1667 = ORIENTED_EDGE ( 'NONE', *, *, #2961, .F. ) ;
#1668 = PRODUCT ( 'torque disk', 'torque disk', '', ( #950 ) ) ;
#1669 = EDGE_CURVE ( 'NONE', #597, #1031, #1681, .T. ) ;
#1670 = DIRECTION ( 'NONE',  ( -0.000000000000000000, -0.000000000000000000, 1.000000000000000000 ) ) ;
#1671 = LINE ( 'NONE', #3523, #2089 ) ;
#1672 = EDGE_LOOP ( 'NONE', ( #3004, #3131, #3882, #3418 ) ) ;
#1673 = EDGE_CURVE ( 'NONE', #2240, #4310, #2429, .T. ) ;
#1674 = AXIS2_PLACEMENT_3D ( 'NONE', #2784, #3621, #2030 ) ;
#1675 = CARTESIAN_POINT ( 'NONE',  ( 2.500000000000000000, 1.178949249685213863, -2.042000000000001148 ) ) ;
#1676 = SURFACE_SIDE_STYLE ('',( #4379 ) ) ;
#1677 = CARTESIAN_POINT ( 'NONE',  ( 0.000000000000000000, 0.000000000000000000, 4.000000000000000000 ) ) ;
#1678 = CARTESIAN_POINT ( 'NONE',  ( -23.68543856465402442, -8.000000000000003553, 14.30577747056276472 ) ) ;
#1679 = ORIENTED_EDGE ( 'NONE', *, *, #3629, .F. ) ;
#1680 = VERTEX_POINT ( 'NONE', #559 ) ;
#1681 = LINE ( 'NONE', #185, #1934 ) ;
#1682 = AXIS2_PLACEMENT_3D ( 'NONE', #532, #459, #2057 ) ;
#1683 = CARTESIAN_POINT ( 'NONE',  ( 4.000000000000003553, 0.000000000000000000, 0.000000000000000000 ) ) ;
#1684 = PLANE ( 'NONE',  #979 ) ;
#1685 = ORIENTED_EDGE ( 'NONE', *, *, #2751, .T. ) ;
#1686 = AXIS2_PLACEMENT_3D ( 'NONE', #4693, #2800, #3128 ) ;
#1687 = ORIENTED_EDGE ( 'NONE', *, *, #4298, .T. ) ;
#1688 = SHAPE_REPRESENTATION_RELATIONSHIP ( 'NONE' , 'NONE' ,  #4221, #755 ) ;
#1689 = CARTESIAN_POINT ( 'NONE',  ( 5.000000000000000888, 0.000000000000000000, 0.000000000000000000 ) ) ;
#1690 = DIRECTION ( 'NONE',  ( -1.000000000000000000, 0.000000000000000000, 0.000000000000000000 ) ) ;
#1691 = VECTOR ( 'NONE', #731, 1000.000000000000000 ) ;
#1692 = DIRECTION ( 'NONE',  ( -1.000000000000000000, -0.000000000000000000, -0.000000000000000000 ) ) ;
#1693 = EDGE_CURVE ( 'NONE', #2856, #1150, #2104, .T. ) ;
#1694 = EDGE_CURVE ( 'NONE', #3027, #497, #14, .T. ) ;
#1695 = VERTEX_POINT ( 'NONE', #3246 ) ;
#1696 = AXIS2_PLACEMENT_3D ( 'NONE', #4526, #1055, #2994 ) ;
#1697 = DIRECTION ( 'NONE',  ( 1.357798298438996130E-15, -1.000000000000000000, 0.000000000000000000 ) ) ;
#1698 = DIRECTION ( 'NONE',  ( 4.073394895316987600E-15, -1.000000000000000000, 0.000000000000000000 ) ) ;
#1699 = CIRCLE ( 'NONE', #737, 2.099999999999990763 ) ;
#1700 = AXIS2_PLACEMENT_3D ( 'NONE', #918, #2142, #4815 ) ;
#1701 = VECTOR ( 'NONE', #1541, 1000.000000000000000 ) ;
#1702 = EDGE_LOOP ( 'NONE', ( #2064, #1591, #562, #795 ) ) ;
#1703 = EDGE_CURVE ( 'NONE', #987, #3261, #1446, .T. ) ;
#1704 = VECTOR ( 'NONE', #455, 1000.000000000000000 ) ;
#1705 = FACE_OUTER_BOUND ( 'NONE', #1312, .T. ) ;
#1706 = EDGE_CURVE ( 'NONE', #4182, #115, #981, .T. ) ;
#1707 = VERTEX_POINT ( 'NONE', #4770 ) ;
#1708 = ORIENTED_EDGE ( 'NONE', *, *, #3725, .F. ) ;
#1709 = DIRECTION ( 'NONE',  ( 0.000000000000000000, 0.000000000000000000, -1.000000000000000000 ) ) ;
#1710 = PLANE ( 'NONE',  #4164 ) ;
#1711 = CARTESIAN_POINT ( 'NONE',  ( -21.37171027316247063, 8.500000000000072831, -12.00000000000000000 ) ) ;
#1712 = ORIENTED_EDGE ( 'NONE', *, *, #3804, .F. ) ;
#1713 = DIRECTION ( 'NONE',  ( 0.000000000000000000, 0.000000000000000000, -1.000000000000000000 ) ) ;
#1714 = CARTESIAN_POINT ( 'NONE',  ( 0.000000000000000000, 0.000000000000000000, -32.00000000000000000 ) ) ;
#1715 = VECTOR ( 'NONE', #2134, 1000.000000000000114 ) ;
#1716 = VERTEX_POINT ( 'NONE', #1334 ) ;
#1717 = CARTESIAN_POINT ( 'NONE',  ( 0.1999999999999987899, 4.286263797015736595E-16, -3.500000000000000000 ) ) ;
#1718 = CYLINDRICAL_SURFACE ( 'NONE', #801, 2.649999999999992806 ) ;
#1719 = ORIENTED_EDGE ( 'NONE', *, *, #1693, .T. ) ;
#1720 = DIRECTION ( 'NONE',  ( 0.000000000000000000, 0.000000000000000000, -1.000000000000000000 ) ) ;
#1721 = ADVANCED_FACE ( 'NONE', ( #3283 ), #3453, .T. ) ;
#1722 = VERTEX_POINT ( 'NONE', #4383 ) ;
#1723 = APPLICATION_CONTEXT ( 'automotive_design' ) ;
#1724 = EDGE_CURVE ( 'NONE', #3915, #1400, #3539, .T. ) ;
#1725 = ADVANCED_FACE ( 'NONE', ( #2917 ), #3632, .T. ) ;
#1726 = ADVANCED_FACE ( 'NONE', ( #4005 ), #1657, .F. ) ;
#1727 = DIRECTION ( 'NONE',  ( -1.000000000000000000, -0.000000000000000000, -0.000000000000000000 ) ) ;
#1728 = DIRECTION ( 'NONE',  ( 1.000000000000000000, -0.000000000000000000, -0.000000000000000000 ) ) ;
#1729 = DIRECTION ( 'NONE',  ( -4.336808689942018722E-16, -1.000000000000000000, 0.000000000000000000 ) ) ;
#1730 = ORIENTED_EDGE ( 'NONE', *, *, #2961, .T. ) ;
#1731 = VERTEX_POINT ( 'NONE', #4712 ) ;
#1732 =( LENGTH_UNIT ( ) NAMED_UNIT ( * ) SI_UNIT ( .MILLI., .METRE. ) );
#1733 = DIRECTION ( 'NONE',  ( -0.7071067811865359154, 0.000000000000000000, 0.7071067811865591191 ) ) ;
#1734 = DIRECTION ( 'NONE',  ( -0.000000000000000000, 1.000000000000000000, 1.224646799147353207E-16 ) ) ;
#1735 = FACE_OUTER_BOUND ( 'NONE', #1170, .T. ) ;
#1736 = EDGE_LOOP ( 'NONE', ( #2085, #3107, #889, #2894, #3323, #3821, #3521, #1708 ) ) ;
#1737 = CYLINDRICAL_SURFACE ( 'NONE', #2828, 2.099999999999994316 ) ;
#1738 = DIRECTION ( 'NONE',  ( 0.000000000000000000, 0.000000000000000000, 1.000000000000000000 ) ) ;
#1739 = CARTESIAN_POINT ( 'NONE',  ( 22.21307774062919194, -11.47223234890554266, -31.94772731936956944 ) ) ;
#1740 = ORIENTED_EDGE ( 'NONE', *, *, #1107, .T. ) ;
#1741 = CARTESIAN_POINT ( 'NONE',  ( 0.000000000000000000, -0.8865213383406690406, 1.535500000000000975 ) ) ;
#1742 = SHAPE_DEFINITION_REPRESENTATION ( #3097, #1644 ) ;
#1743 = SURFACE_SIDE_STYLE ('',( #2322 ) ) ;
#1744 = ORIENTED_EDGE ( 'NONE', *, *, #986, .T. ) ;
#1745 = EDGE_CURVE ( 'NONE', #2165, #2366, #4250, .T. ) ;
#1746 = ADVANCED_FACE ( 'NONE', ( #154 ), #2118, .T. ) ;
#1747 = DIRECTION ( 'NONE',  ( 0.000000000000000000, 0.4999999999999993339, -0.8660254037844390407 ) ) ;
#1748 = FACE_OUTER_BOUND ( 'NONE', #3830, .T. ) ;
#1749 = VECTOR ( 'NONE', #4469, 1000.000000000000000 ) ;
#1750 = DIRECTION ( 'NONE',  ( -0.000000000000000000, -0.000000000000000000, 1.000000000000000000 ) ) ;
#1751 = ORIENTED_EDGE ( 'NONE', *, *, #1883, .T. ) ;
#1752 = AXIS2_PLACEMENT_3D ( 'NONE', #3724, #13, #4466 ) ;
#1753 = ORIENTED_EDGE ( 'NONE', *, *, #4263, .T. ) ;
#1754 = CARTESIAN_POINT ( 'NONE',  ( 0.000000000000000000, 0.000000000000000000, 0.000000000000000000 ) ) ;
#1755 = CARTESIAN_POINT ( 'NONE',  ( -9.999999999999975131, -16.00000000000000000, -26.00000000000000355 ) ) ;
#1756 = CARTESIAN_POINT ( 'NONE',  ( 25.00000000000000000, -11.10102051443364068, -31.00000000000000000 ) ) ;
#1757 = FACE_OUTER_BOUND ( 'NONE', #3032, .T. ) ;
#1758 = EDGE_CURVE ( 'NONE', #3948, #1323, #4813, .T. ) ;
#1759 = VECTOR ( 'NONE', #1837, 1000.000000000000000 ) ;
#1760 = EDGE_LOOP ( 'NONE', ( #189, #4344, #367, #1298 ) ) ;
#1761 = FACE_OUTER_BOUND ( 'NONE', #2254, .T. ) ;
#1762 = CARTESIAN_POINT ( 'NONE',  ( 25.00000000000000000, 0.000000000000000000, -20.00000000000000000 ) ) ;
#1763 = VECTOR ( 'NONE', #80, 1000.000000000000000 ) ;
#1764 = LINE ( 'NONE', #168, #1840 ) ;
#1765 = AXIS2_PLACEMENT_3D ( 'NONE', #4794, #237, #587 ) ;
#1766 = EDGE_LOOP ( 'NONE', ( #380, #3790, #3447, #3166 ) ) ;
#1767 = CIRCLE ( 'NONE', #2255, 2.041999999999999815 ) ;
#1768 = CIRCLE ( 'NONE', #4649, 22.99999999999998934 ) ;
#1769 = DIRECTION ( 'NONE',  ( -0.000000000000000000, -0.000000000000000000, 1.000000000000000000 ) ) ;
#1770 = DIRECTION ( 'NONE',  ( -1.000000000000000000, -0.000000000000000000, -0.000000000000000000 ) ) ;
#1771 = AXIS2_PLACEMENT_3D ( 'NONE', #1080, #4914, #3476 ) ;
#1772 = VECTOR ( 'NONE', #1747, 1000.000000000000000 ) ;
#1773 = CARTESIAN_POINT ( 'NONE',  ( 0.000000000000000000, 0.000000000000000000, -1.999999999999994893 ) ) ;
#1774 = PRODUCT_DEFINITION_SHAPE ( 'NONE', 'NONE',  #2896 ) ;
#1775 = ORIENTED_EDGE ( 'NONE', *, *, #323, .T. ) ;
#1776 = AXIS2_PLACEMENT_3D ( 'NONE', #330, #1902, #1476 ) ;
#1777 = AXIS2_PLACEMENT_3D ( 'NONE', #2052, #1294, #4320 ) ;
#1778 = DIRECTION ( 'NONE',  ( 0.000000000000000000, -0.4999999999999990563, 0.8660254037844391517 ) ) ;
#1779 = DIRECTION ( 'NONE',  ( 1.000000000000000000, 0.000000000000000000, 0.000000000000000000 ) ) ;
#1780 = CIRCLE ( 'NONE', #3547, 23.00000000000000711 ) ;
#1781 = DIRECTION ( 'NONE',  ( 1.000000000000000000, -0.000000000000000000, -0.000000000000000000 ) ) ;
#1782 = EDGE_LOOP ( 'NONE', ( #55, #4725, #4647, #30 ) ) ;
#1783 = CIRCLE ( 'NONE', #2761, 25.00000000000000000 ) ;
#1784 = EDGE_CURVE ( 'NONE', #1327, #2708, #902, .T. ) ;
#1785 = CARTESIAN_POINT ( 'NONE',  ( -9.999999999999975131, -16.00000000000000000, -26.00000000000000355 ) ) ;
#1786 = CARTESIAN_POINT ( 'NONE',  ( 0.000000000000000000, 0.000000000000000000, -12.00000000000000000 ) ) ;
#1787 = EDGE_CURVE ( 'NONE', #1889, #2416, #3385, .T. ) ;
#1788 = EDGE_LOOP ( 'NONE', ( #4680, #2042, #2561 ) ) ;
#1789 = CARTESIAN_POINT ( 'NONE',  ( 2.000000000000000000, 0.8865213383406685965, -1.535500000000000753 ) ) ;
#1790 = ORIENTED_EDGE ( 'NONE', *, *, #765, .T. ) ;
#1791 = AXIS2_PLACEMENT_3D ( 'NONE', #2409, #447, #1528 ) ;
#1792 = ORIENTED_EDGE ( 'NONE', *, *, #1415, .T. ) ;
#1793 = CARTESIAN_POINT ( 'NONE',  ( 23.61000000000001364, 0.000000000000000000, 0.000000000000000000 ) ) ;
#1794 = DIRECTION ( 'NONE',  ( 1.000000000000000000, -0.000000000000000000, -0.000000000000000000 ) ) ;
#1795 = CIRCLE ( 'NONE', #3008, 2.041999999999999815 ) ;
#1796 = CARTESIAN_POINT ( 'NONE',  ( 0.2500000000000002220, 0.000000000000000000, 0.000000000000000000 ) ) ;
#1797 = ADVANCED_FACE ( 'NONE', ( #3358 ), #4407, .F. ) ;
#1798 =( REPRESENTATION_RELATIONSHIP ('NONE','NONE', #137, #1644 ) REPRESENTATION_RELATIONSHIP_WITH_TRANSFORMATION ( #2013 )SHAPE_REPRESENTATION_RELATIONSHIP( ) );
#1799 = EDGE_LOOP ( 'NONE', ( #4029, #4890, #424, #1186 ) ) ;
#1800 = UNCERTAINTY_MEASURE_WITH_UNIT (LENGTH_MEASURE( 1.000000000000000082E-05 ), #4904, 'distance_accuracy_value', 'NONE');
#1801 = CYLINDRICAL_SURFACE ( 'NONE', #2637, 25.00000000000000000 ) ;
#1802 = CARTESIAN_POINT ( 'NONE',  ( -19.30673457630776824, 12.50000000000006750, -4.000000000000000000 ) ) ;
#1803 = LINE ( 'NONE', #3332, #2185 ) ;
#1804 = EDGE_LOOP ( 'NONE', ( #1416, #4432, #4933, #2635 ) ) ;
#1805 = CARTESIAN_POINT ( 'NONE',  ( 22.82142399877221095, 10.20738559227135944, -24.38442231784400249 ) ) ;
#1806 = LINE ( 'NONE', #4915, #3853 ) ;
#1807 = CARTESIAN_POINT ( 'NONE',  ( 2.500000000000000000, -2.629050547790028551E-15, -2.041999999999999815 ) ) ;
#1808 = ORIENTED_EDGE ( 'NONE', *, *, #1240, .F. ) ;
#1809 = DIRECTION ( 'NONE',  ( -1.000000000000000000, 0.000000000000000000, 0.000000000000000000 ) ) ;
#1810 =( NAMED_UNIT ( * ) SI_UNIT ( $, .STERADIAN. ) SOLID_ANGLE_UNIT ( ) );
#1811 = DIRECTION ( 'NONE',  ( -1.000000000000000000, 0.000000000000000000, -0.000000000000000000 ) ) ;
#1812 = DIRECTION ( 'NONE',  ( 0.000000000000000000, 0.000000000000000000, -1.000000000000000000 ) ) ;
#1813 = ORIENTED_EDGE ( 'NONE', *, *, #849, .F. ) ;
#1814 = CARTESIAN_POINT ( 'NONE',  ( 2.444036937190193033E-14, 6.999999999999999112, -32.00000000000000000 ) ) ;
#1815 = ORIENTED_EDGE ( 'NONE', *, *, #3196, .F. ) ;
#1816 = DIRECTION ( 'NONE',  ( -1.357798298438996130E-15, 1.000000000000000000, 0.000000000000000000 ) ) ;
#1817 = CYLINDRICAL_SURFACE ( 'NONE', #882, 5.999999999999998224 ) ;
#1818 = DIRECTION ( 'NONE',  ( 1.000000000000000000, 5.329070518200750605E-15, 0.000000000000000000 ) ) ;
#1819 = VERTEX_POINT ( 'NONE', #4861 ) ;
#1820 = EDGE_CURVE ( 'NONE', #467, #941, #3375, .T. ) ;
#1821 =( GEOMETRIC_REPRESENTATION_CONTEXT ( 3 ) GLOBAL_UNCERTAINTY_ASSIGNED_CONTEXT ( ( #4602 ) ) GLOBAL_UNIT_ASSIGNED_CONTEXT ( ( #3420, #10, #3813 ) ) REPRESENTATION_CONTEXT ( 'NONE', 'WORKASPACE' ) );
#1822 = LINE ( 'NONE', #2531, #4714 ) ;
#1823 = CARTESIAN_POINT ( 'NONE',  ( -9.999999999999975131, -16.00000000000000000, -23.90000000000000568 ) ) ;
#1824 = DIRECTION ( 'NONE',  ( 1.000000000000000000, 0.000000000000000000, -0.000000000000000000 ) ) ;
#1825 = EDGE_LOOP ( 'NONE', ( #726, #3795, #3963 ) ) ;
#1826 = DIRECTION ( 'NONE',  ( 1.000000000000000000, -0.000000000000000000, -0.000000000000000000 ) ) ;
#1827 = LINE ( 'NONE', #1402, #96 ) ;
#1828 = ORIENTED_EDGE ( 'NONE', *, *, #2472, .F. ) ;
#1829 = AXIS2_PLACEMENT_3D ( 'NONE', #429, #4625, #2380 ) ;
#1830 = DIRECTION ( 'NONE',  ( -1.000000000000000000, -0.000000000000000000, -0.000000000000000000 ) ) ;
#1831 = CARTESIAN_POINT ( 'NONE',  ( 2.000000000000000000, 0.000000000000000000, 1.535500000000000087 ) ) ;
#1832 = CARTESIAN_POINT ( 'NONE',  ( 2.000000000000000000, 0.8865213383406717051, 1.535499999999998533 ) ) ;
#1833 = ORIENTED_EDGE ( 'NONE', *, *, #1510, .F. ) ;
#1834 = CIRCLE ( 'NONE', #2324, 22.99999999999998934 ) ;
#1835 = PLANE ( 'NONE',  #3774 ) ;
#1836 = DIRECTION ( 'NONE',  ( 0.000000000000000000, 0.000000000000000000, -1.000000000000000000 ) ) ;
#1837 = DIRECTION ( 'NONE',  ( -0.000000000000000000, -0.000000000000000000, 1.000000000000000000 ) ) ;
#1838 = PRODUCT_DEFINITION_SHAPE ( 'NONE', 'NONE',  #4972 ) ;
#1839 = EDGE_CURVE ( 'NONE', #2615, #2974, #1054, .T. ) ;
#1840 = VECTOR ( 'NONE', #4831, 1000.000000000000000 ) ;
#1841 = EDGE_LOOP ( 'NONE', ( #4765, #591, #2669, #1744, #616 ) ) ;
#1842 = CIRCLE ( 'NONE', #4646, 5.999999999999998224 ) ;
#1843 = LINE ( 'NONE', #4804, #3994 ) ;
#1844 =( NAMED_UNIT ( * ) PLANE_ANGLE_UNIT ( ) SI_UNIT ( $, .RADIAN. ) );
#1845 = CYLINDRICAL_SURFACE ( 'NONE', #4582, 2.000000000000000888 ) ;
#1846 = ADVANCED_FACE ( 'NONE', ( #3335 ), #2631, .F. ) ;
#1847 = VECTOR ( 'NONE', #134, 1000.000000000000000 ) ;
#1848 = AXIS2_PLACEMENT_3D ( 'NONE', #1785, #1560, #410 ) ;
#1849 = ORIENTED_EDGE ( 'NONE', *, *, #3355, .T. ) ;
#1850 = AXIS2_PLACEMENT_3D ( 'NONE', #1007, #3965, #2141 ) ;
#1851 = AXIS2_PLACEMENT_3D ( 'NONE', #2301, #401, #1927 ) ;
#1852 = PLANE ( 'NONE',  #2825 ) ;
#1853 = ADVANCED_FACE ( 'NONE', ( #4885, #2557 ), #1852, .F. ) ;
#1854 = DIRECTION ( 'NONE',  ( 1.000000000000000000, -0.000000000000000000, -0.000000000000000000 ) ) ;
#1855 = FACE_OUTER_BOUND ( 'NONE', #1841, .T. ) ;
#1856 = PLANE ( 'NONE',  #1453 ) ;
#1857 = VECTOR ( 'NONE', #1522, 1000.000000000000000 ) ;
#1858 = CIRCLE ( 'NONE', #17, 23.00000000000000711 ) ;
#1859 = ORIENTED_EDGE ( 'NONE', *, *, #172, .F. ) ;
#1860 = PLANE ( 'NONE',  #1393 ) ;
#1861 = DIRECTION ( 'NONE',  ( 1.000000000000000000, 0.000000000000000000, 0.000000000000000000 ) ) ;
#1862 = LINE ( 'NONE', #1482, #1943 ) ;
#1863 = LINE ( 'NONE', #2567, #1542 ) ;
#1864 = ORIENTED_EDGE ( 'NONE', *, *, #1396, .F. ) ;
#1865 = AXIS2_PLACEMENT_3D ( 'NONE', #1342, #2802, #3617 ) ;
#1866 = CARTESIAN_POINT ( 'NONE',  ( 0.000000000000000000, 0.000000000000000000, -20.00000000000000000 ) ) ;
#1867 = DIRECTION ( 'NONE',  ( 1.000000000000000000, -0.000000000000000000, -0.000000000000000000 ) ) ;
#1868 = SURFACE_STYLE_USAGE ( .BOTH. , #1003 ) ;
#1869 = ORIENTED_EDGE ( 'NONE', *, *, #234, .T. ) ;
#1870 = AXIS2_PLACEMENT_3D ( 'NONE', #2169, #2968, #4529 ) ;
#1871 = ADVANCED_FACE ( 'NONE', ( #4107 ), #1448, .F. ) ;
#1872 = CARTESIAN_POINT ( 'NONE',  ( -6.708203932499367639, 2.000000000000001332, -32.00000000000000000 ) ) ;
#1873 = DIRECTION ( 'NONE',  ( 0.000000000000000000, 0.000000000000000000, -1.000000000000000000 ) ) ;
#1874 = AXIS2_PLACEMENT_3D ( 'NONE', #1492, #2227, #3727 ) ;
#1875 = VERTEX_POINT ( 'NONE', #3406 ) ;
#1876 = UNCERTAINTY_MEASURE_WITH_UNIT (LENGTH_MEASURE( 1.000000000000000082E-05 ), #4184, 'distance_accuracy_value', 'NONE');
#1877 = EDGE_CURVE ( 'NONE', #1320, #3389, #2992, .T. ) ;
#1878 = CARTESIAN_POINT ( 'NONE',  ( 22.31144310522464735, 11.28096319364322042, -22.27413919560993705 ) ) ;
#1879 = DIRECTION ( 'NONE',  ( -1.000000000000000000, 0.000000000000000000, 0.000000000000000000 ) ) ;
#1880 = DIRECTION ( 'NONE',  ( 0.000000000000000000, 0.000000000000000000, -1.000000000000000000 ) ) ;
#1881 = PLANE ( 'NONE',  #4575 ) ;
#1882 = ORIENTED_EDGE ( 'NONE', *, *, #3560, .F. ) ;
#1883 = EDGE_CURVE ( 'NONE', #3363, #2945, #2587, .T. ) ;
#1884 = EDGE_CURVE ( 'NONE', #4842, #3993, #624, .T. ) ;
#1885 = CARTESIAN_POINT ( 'NONE',  ( 2.000000000000000000, 1.773042676681340968, -2.276824562219559311E-15 ) ) ;
#1886 = DIRECTION ( 'NONE',  ( -1.000000000000000000, 0.000000000000000000, 0.000000000000000000 ) ) ;
#1887 = PLANE ( 'NONE',  #3137 ) ;
#1888 = CARTESIAN_POINT ( 'NONE',  ( 21.94848156259736527, 11.96939725984945113, -31.50629648535032601 ) ) ;
#1889 = VERTEX_POINT ( 'NONE', #698 ) ;
#1890 = ADVANCED_FACE ( 'NONE', ( #258 ), #3730, .T. ) ;
#1891 = APPLICATION_CONTEXT ( 'automotive_design' ) ;
#1892 = DIRECTION ( 'NONE',  ( 0.000000000000000000, 0.000000000000000000, 1.000000000000000000 ) ) ;
#1893 = CARTESIAN_POINT ( 'NONE',  ( 2.000000000000000000, -0.8865213383406690406, 1.535500000000000975 ) ) ;
#1894 = ORIENTED_EDGE ( 'NONE', *, *, #1217, .F. ) ;
#1895 = UNCERTAINTY_MEASURE_WITH_UNIT (LENGTH_MEASURE( 1.000000000000000082E-05 ), #3470, 'distance_accuracy_value', 'NONE');
#1896 = DIRECTION ( 'NONE',  ( 1.000000000000000000, -1.106769389831504682E-16, 0.000000000000000000 ) ) ;
#1897 = CARTESIAN_POINT ( 'NONE',  ( -13.99999999999993250, -16.00000000000000000, -26.00000000000000355 ) ) ;
#1898 = ORIENTED_EDGE ( 'NONE', *, *, #2997, .F. ) ;
#1899 = ORIENTED_EDGE ( 'NONE', *, *, #966, .F. ) ;
#1900 = CARTESIAN_POINT ( 'NONE',  ( 23.61000000000001364, 0.000000000000000000, 2.000000000000000444 ) ) ;
#1901 = FACE_OUTER_BOUND ( 'NONE', #735, .T. ) ;
#1902 = DIRECTION ( 'NONE',  ( -1.000000000000000000, -0.000000000000000000, -0.000000000000000000 ) ) ;
#1903 = EDGE_CURVE ( 'NONE', #1923, #3747, #2500, .T. ) ;
#1904 = ORIENTED_EDGE ( 'NONE', *, *, #1187, .T. ) ;
#1905 = AXIS2_PLACEMENT_3D ( 'NONE', #3098, #2715, #4229 ) ;
#1906 = CYLINDRICAL_SURFACE ( 'NONE', #1791, 4.250000000000000000 ) ;
#1907 = DIRECTION ( 'NONE',  ( 0.5150380749100550437, 1.049727191138617956E-16, 0.8571673007021117785 ) ) ;
#1908 = CARTESIAN_POINT ( 'NONE',  ( 2.000000000000000000, 1.773042676681340968, -2.276824562219559311E-15 ) ) ;
#1909 = CARTESIAN_POINT ( 'NONE',  ( 0.000000000000000000, 0.000000000000000000, -12.00000000000000000 ) ) ;
#1910 = EDGE_CURVE ( 'NONE', #3903, #4259, #1473, .T. ) ;
#1911 = ORIENTED_EDGE ( 'NONE', *, *, #3354, .T. ) ;
#1912 = VERTEX_POINT ( 'NONE', #4524 ) ;
#1913 = VECTOR ( 'NONE', #3743, 1000.000000000000000 ) ;
#1914 = ORIENTED_EDGE ( 'NONE', *, *, #4729, .T. ) ;
#1915 = CARTESIAN_POINT ( 'NONE',  ( 25.00000000000000000, -11.80087472665740478, -30.28571428571428470 ) ) ;
#1916 = SURFACE_STYLE_FILL_AREA ( #2295 ) ;
#1917 = EDGE_CURVE ( 'NONE', #4866, #4838, #2755, .T. ) ;
#1918 = AXIS2_PLACEMENT_3D ( 'NONE', #1146, #2700, #1115 ) ;
#1919 = VERTEX_POINT ( 'NONE', #771 ) ;
#1920 = DIRECTION ( 'NONE',  ( -0.000000000000000000, -0.000000000000000000, 1.000000000000000000 ) ) ;
#1921 = DIRECTION ( 'NONE',  ( 1.000000000000000000, -0.000000000000000000, -0.000000000000000000 ) ) ;
#1922 = AXIS2_PLACEMENT_3D ( 'NONE', #1255, #1275, #1648 ) ;
#1923 = VERTEX_POINT ( 'NONE', #4177 ) ;
#1924 = ORIENTED_EDGE ( 'NONE', *, *, #4606, .F. ) ;
#1925 = VECTOR ( 'NONE', #3158, 1000.000000000000000 ) ;
#1926 = CIRCLE ( 'NONE', #4732, 4.250000000000000000 ) ;
#1927 = DIRECTION ( 'NONE',  ( 0.000000000000000000, 0.000000000000000000, 1.000000000000000000 ) ) ;
#1928 = AXIS2_PLACEMENT_3D ( 'NONE', #779, #1582, #56 ) ;
#1929 = CARTESIAN_POINT ( 'NONE',  ( -16.10609822396473589, 5.440000000000003055, -12.00000000000000000 ) ) ;
#1930 = CARTESIAN_POINT ( 'NONE',  ( 0.000000000000000000, 0.000000000000000000, 12.00000000000000000 ) ) ;
#1931 = CARTESIAN_POINT ( 'NONE',  ( 6.999999999999999112, 0.000000000000000000, -20.00000000000000000 ) ) ;
#1932 = ORIENTED_EDGE ( 'NONE', *, *, #4474, .T. ) ;
#1933 = CIRCLE ( 'NONE', #4653, 25.00000000000000000 ) ;
#1934 = VECTOR ( 'NONE', #520, 1000.000000000000000 ) ;
#1935 = EDGE_CURVE ( 'NONE', #3401, #3396, #4280, .T. ) ;
#1936 = CARTESIAN_POINT ( 'NONE',  ( 16.42012538500922858, 19.65653790321621130, 26.00000000000000000 ) ) ;
#1937 = CARTESIAN_POINT ( 'NONE',  ( 15.00000000000000000, 20.00000000000000355, -32.00000000000000000 ) ) ;
#1938 = CARTESIAN_POINT ( 'NONE',  ( -1.387778780781444295E-15, 4.108768631691174362E-15, -12.00000000000000000 ) ) ;
#1939 = AXIS2_PLACEMENT_3D ( 'NONE', #2200, #3006, #3397 ) ;
#1940 = DIRECTION ( 'NONE',  ( 1.357798298438996130E-15, -1.000000000000000000, 0.000000000000000000 ) ) ;
#1941 = AXIS2_PLACEMENT_3D ( 'NONE', #2098, #4824, #4038 ) ;
#1942 = ORIENTED_EDGE ( 'NONE', *, *, #3742, .T. ) ;
#1943 = VECTOR ( 'NONE', #4114, 1000.000000000000000 ) ;
#1944 = ORIENTED_EDGE ( 'NONE', *, *, #4769, .T. ) ;
#1945 = EDGE_CURVE ( 'NONE', #3993, #4372, #49, .T. ) ;
#1946 = LINE ( 'NONE', #4239, #407 ) ;
#1947 = CARTESIAN_POINT ( 'NONE',  ( 15.00000000000000000, -20.00000000000000355, -20.00000000000000000 ) ) ;
#1948 = DIRECTION ( 'NONE',  ( 1.000000000000000000, -0.000000000000000000, -0.000000000000000000 ) ) ;
#1949 = AXIS2_PLACEMENT_3D ( 'NONE', #163, #2126, #893 ) ;
#1950 = ORIENTED_EDGE ( 'NONE', *, *, #3295, .T. ) ;
#1951 = EDGE_CURVE ( 'NONE', #2597, #3217, #2035, .T. ) ;
#1952 = ADVANCED_FACE ( 'NONE', ( #4550 ), #1128, .T. ) ;
#1953 = CARTESIAN_POINT ( 'NONE',  ( 12.50000000000000000, -1.383461737289380927E-15, 12.00000000000000000 ) ) ;
#1954 = VECTOR ( 'NONE', #3101, 1000.000000000000000 ) ;
#1955 = CARTESIAN_POINT ( 'NONE',  ( -6.537332342993324937E-14, 16.00000000000000000, -28.10000000000000142 ) ) ;
#1956 = ORIENTED_EDGE ( 'NONE', *, *, #4263, .F. ) ;
#1957 = ORIENTED_EDGE ( 'NONE', *, *, #3902, .F. ) ;
#1958 = PRESENTATION_LAYER_ASSIGNMENT (  '', '', ( #2202 ) ) ;
#1959 = CARTESIAN_POINT ( 'NONE',  ( 22.18564505841181855, 11.52792329777113345, -30.01827759558031161 ) ) ;
#1960 = DIRECTION ( 'NONE',  ( 0.000000000000000000, 0.000000000000000000, -1.000000000000000000 ) ) ;
#1961 = LINE ( 'NONE', #466, #3689 ) ;
#1962 = ORIENTED_EDGE ( 'NONE', *, *, #3675, .T. ) ;
#1963 = ORIENTED_EDGE ( 'NONE', *, *, #4785, .F. ) ;
#1964 = PLANE ( 'NONE',  #257 ) ;
#1965 = DIRECTION ( 'NONE',  ( -0.000000000000000000, -0.000000000000000000, 1.000000000000000000 ) ) ;
#1966 = LINE ( 'NONE', #3789, #1954 ) ;
#1967 = ORIENTED_EDGE ( 'NONE', *, *, #907, .T. ) ;
#1968 = VERTEX_POINT ( 'NONE', #2083 ) ;
#1969 = CARTESIAN_POINT ( 'NONE',  ( 6.517431832507181422E-14, -16.00000000000000000, -28.10000000000000142 ) ) ;
#1970 = DIRECTION ( 'NONE',  ( 1.000000000000000000, 0.000000000000000000, 0.000000000000000000 ) ) ;
#1971 = CARTESIAN_POINT ( 'NONE',  ( 0.000000000000000000, 0.000000000000000000, -32.00000000000000000 ) ) ;
#1972 = ORIENTED_EDGE ( 'NONE', *, *, #133, .F. ) ;
#1973 = CARTESIAN_POINT ( 'NONE',  ( 0.000000000000000000, 0.000000000000000000, -4.000000000000000000 ) ) ;
#1974 = CARTESIAN_POINT ( 'NONE',  ( 2.500000000000000000, -1.768423874527823791, -1.020999999999998353 ) ) ;
#1975 = ORIENTED_EDGE ( 'NONE', *, *, #808, .F. ) ;
#1976 = EDGE_CURVE ( 'NONE', #2919, #3988, #3649, .T. ) ;
#1977 = ORIENTED_EDGE ( 'NONE', *, *, #4367, .F. ) ;
#1978 = PRODUCT_DEFINITION_CONTEXT ( 'detailed design', #609, 'design' ) ;
#1979 = CARTESIAN_POINT ( 'NONE',  ( 22.31344532614782850, 11.27701289969359166, -29.72101288460549284 ) ) ;
#1980 = FACE_OUTER_BOUND ( 'NONE', #2776, .T. ) ;
#1981 = LINE ( 'NONE', #3487, #1615 ) ;
#1982 = EDGE_CURVE ( 'NONE', #3321, #3988, #2661, .T. ) ;
#1983 = ORIENTED_EDGE ( 'NONE', *, *, #3211, .F. ) ;
#1984 = ORIENTED_EDGE ( 'NONE', *, *, #1574, .F. ) ;
#1985 = DIRECTION ( 'NONE',  ( 1.000000000000000000, 0.000000000000000000, 0.000000000000000000 ) ) ;
#1986 = DIRECTION ( 'NONE',  ( 0.000000000000000000, -1.224646799147353207E-16, 1.000000000000000000 ) ) ;
#1987 = CARTESIAN_POINT ( 'NONE',  ( 21.94848156259736527, -11.96939725984945468, -20.49370351464968465 ) ) ;
#1988 = ORIENTED_EDGE ( 'NONE', *, *, #3262, .F. ) ;
#1989 = VERTEX_POINT ( 'NONE', #2482 ) ;
#1990 = PRESENTATION_STYLE_ASSIGNMENT (( #139 ) ) ;
#1991 = CARTESIAN_POINT ( 'NONE',  ( 2.500000000000000000, 0.000000000000000000, 0.000000000000000000 ) ) ;
#1992 = CARTESIAN_POINT ( 'NONE',  ( 0.000000000000000000, 0.000000000000000000, -12.00000000000000000 ) ) ;
#1993 = DIRECTION ( 'NONE',  ( 1.000000000000000000, 0.000000000000000000, 0.000000000000000000 ) ) ;
#1994 = ORIENTED_EDGE ( 'NONE', *, *, #4912, .T. ) ;
#1995 = CARTESIAN_POINT ( 'NONE',  ( 0.000000000000000000, 0.000000000000000000, 14.30577747056276472 ) ) ;
#1996 = EDGE_CURVE ( 'NONE', #54, #4892, #511, .T. ) ;
#1997 = CARTESIAN_POINT ( 'NONE',  ( 15.00000000000000178, 16.00000000000000000, -23.35000000000001563 ) ) ;
#1998 = ORIENTED_EDGE ( 'NONE', *, *, #820, .F. ) ;
#1999 = MANIFOLD_SOLID_BREP ( 'Hex', #2272 ) ;
#2000 = EDGE_LOOP ( 'NONE', ( #1572, #3081, #2766, #1193 ) ) ;
#2001 = PLANE ( 'NONE',  #4429 ) ;
#2002 = PRODUCT_RELATED_PRODUCT_CATEGORY ( 'part', '', ( #1668 ) ) ;
#2003 = EDGE_CURVE ( 'NONE', #1558, #1031, #1653, .T. ) ;
#2004 = CARTESIAN_POINT ( 'NONE',  ( 22.61871848390502393, -10.64917431867735154, -23.27817350896996018 ) ) ;
#2005 = DIRECTION ( 'NONE',  ( -1.000000000000000000, -0.000000000000000000, -0.000000000000000000 ) ) ;
#2006 = CARTESIAN_POINT ( 'NONE',  ( 12.49999999999999822, -19.30673457630782863, 12.00000000000000000 ) ) ;
#2007 = ORIENTED_EDGE ( 'NONE', *, *, #3042, .F. ) ;
#2008 = EDGE_LOOP ( 'NONE', ( #567, #948, #701 ) ) ;
#2009 = MANIFOLD_SOLID_BREP ( 'Hex', #1546 ) ;
#2010 = EDGE_CURVE ( 'NONE', #536, #865, #653, .T. ) ;
#2011 = VECTOR ( 'NONE', #1387, 1000.000000000000000 ) ;
#2012 = ADVANCED_FACE ( 'NONE', ( #1148 ), #4426, .T. ) ;
#2013 = ITEM_DEFINED_TRANSFORMATION ( 'NONE', 'NONE', #1023,  #1918 ) ;
#2014 = CARTESIAN_POINT ( 'NONE',  ( 0.000000000000000000, 1.773042676681340968, -2.276824562219559311E-15 ) ) ;
#2015 = DIRECTION ( 'NONE',  ( 0.000000000000000000, 0.000000000000000000, -1.000000000000000000 ) ) ;
#2016 = LINE ( 'NONE', #1265, #342 ) ;
#2017 = AXIS2_PLACEMENT_3D ( 'NONE', #2890, #4404, #3193 ) ;
#2018 = CIRCLE ( 'NONE', #644, 2.700000000000001066 ) ;
#2019 = ORIENTED_EDGE ( 'NONE', *, *, #174, .F. ) ;
#2020 = VERTEX_POINT ( 'NONE', #3054 ) ;
#2021 =( LENGTH_UNIT ( ) NAMED_UNIT ( * ) SI_UNIT ( .MILLI., .METRE. ) );
#2022 = AXIS2_PLACEMENT_3D ( 'NONE', #3650, #516, #2040 ) ;
#2023 = DIRECTION ( 'NONE',  ( 1.000000000000000000, 0.000000000000000000, 0.000000000000000000 ) ) ;
#2024 = AXIS2_PLACEMENT_3D ( 'NONE', #1401, #1826, #2936 ) ;
#2025 = CARTESIAN_POINT ( 'NONE',  ( 6.517431832507181422E-14, -16.00000000000000000, -26.00000000000000355 ) ) ;
#2026 = CARTESIAN_POINT ( 'NONE',  ( 25.00000000000000000, 2.789133085058098087E-16, -2.055000000000000160 ) ) ;
#2027 = ORIENTED_EDGE ( 'NONE', *, *, #523, .F. ) ;
#2028 = VECTOR ( 'NONE', #1132, 1000.000000000000114 ) ;
#2029 = AXIS2_PLACEMENT_3D ( 'NONE', #370, #3373, #4543 ) ;
#2030 = DIRECTION ( 'NONE',  ( 0.000000000000000000, 0.000000000000000000, -1.000000000000000000 ) ) ;
#2031 = DIRECTION ( 'NONE',  ( 1.000000000000000000, 0.000000000000000000, 0.000000000000000000 ) ) ;
#2032 = SHAPE_REPRESENTATION ( 'Input Clamping Hub Sleeve', ( #1918 ), #305 ) ;
#2033 = PRESENTATION_LAYER_ASSIGNMENT (  '', '', ( #1381 ) ) ;
#2034 = ORIENTED_EDGE ( 'NONE', *, *, #3416, .F. ) ;
#2035 = B_SPLINE_CURVE_WITH_KNOTS ( 'NONE', 3,
 ( #1573, #1206, #748, #1554, #3504, #375, #3429, #4836, #4222, #1597, #3067, #2736, #2363, #72, #3138, #4657, #4583, #1158, #1234, #2004, #855, #2767, #486, #3532, #104 ),
 .UNSPECIFIED., .F., .F.,
 ( 4, 2, 2, 2, 2, 2, 1, 2, 2, 2, 2, 2, 4 ),
 ( 0.005424949174462418561, 0.006631086198200497259, 0.007234154710069534006, 0.007837223221938570752, 0.009043360245676652920, 0.009646428757545694871, 0.01024949726941473509, 0.01085256578128377530, 0.01145563429315281552, 0.01266177131689090810, 0.01326483982875994831, 0.01386790834062898853, 0.01507404536436706896 ),
 .UNSPECIFIED. ) ;
#2036 = ORIENTED_EDGE ( 'NONE', *, *, #2816, .T. ) ;
#2037 = FACE_OUTER_BOUND ( 'NONE', #331, .T. ) ;
#2038 = DIRECTION ( 'NONE',  ( 1.000000000000000000, 0.000000000000000000, 0.000000000000000000 ) ) ;
#2039 = LINE ( 'NONE', #3507, #4744 ) ;
#2040 = DIRECTION ( 'NONE',  ( 0.000000000000000000, 0.000000000000000000, -1.000000000000000000 ) ) ;
#2041 = ORIENTED_EDGE ( 'NONE', *, *, #4698, .F. ) ;
#2042 = ORIENTED_EDGE ( 'NONE', *, *, #1273, .T. ) ;
#2043 = AXIS2_PLACEMENT_3D ( 'NONE', #4590, #534, #4557 ) ;
#2044 = LINE ( 'NONE', #2486, #3939 ) ;
#2045 = LINE ( 'NONE', #3100, #1847 ) ;
#2046 = CARTESIAN_POINT ( 'NONE',  ( 23.68543856465402797, 7.999999999999996447, 14.30577747056276472 ) ) ;
#2047 = ADVANCED_FACE ( 'NONE', ( #2702 ), #3815, .T. ) ;
#2048 = ORIENTED_EDGE ( 'NONE', *, *, #3417, .F. ) ;
#2049 = ORIENTED_EDGE ( 'NONE', *, *, #4411, .F. ) ;
#2050 = SURFACE_SIDE_STYLE ('',( #193 ) ) ;
#2051 = CARTESIAN_POINT ( 'NONE',  ( 8.500000000000000000, -21.37171027316251681, 12.00000000000000000 ) ) ;
#2052 = CARTESIAN_POINT ( 'NONE',  ( -31.74999999999995737, 0.000000000000000000, 0.000000000000000000 ) ) ;
#2053 = EDGE_CURVE ( 'NONE', #468, #1580, #3671, .T. ) ;
#2054 = ORIENTED_EDGE ( 'NONE', *, *, #4660, .T. ) ;
#2055 = CARTESIAN_POINT ( 'NONE',  ( -10.00000000000002132, 16.00000000000000000, -28.10000000000000142 ) ) ;
#2056 = CARTESIAN_POINT ( 'NONE',  ( -21.37171027316253102, -8.499999999999925393, -12.00000000000000000 ) ) ;
#2057 = DIRECTION ( 'NONE',  ( 0.000000000000000000, 0.000000000000000000, -1.000000000000000000 ) ) ;
#2058 = MANIFOLD_SOLID_BREP ( 'Boss-Extrude3', #2915 ) ;
#2059 = ORIENTED_EDGE ( 'NONE', *, *, #751, .F. ) ;
#2060 = DIRECTION ( 'NONE',  ( 1.000000000000000000, 0.000000000000000000, 0.000000000000000000 ) ) ;
#2061 = SURFACE_STYLE_USAGE ( .BOTH. , #1676 ) ;
#2062 = FACE_OUTER_BOUND ( 'NONE', #504, .T. ) ;
#2063 = EDGE_LOOP ( 'NONE', ( #1549, #461, #4791, #3172 ) ) ;
#2064 = ORIENTED_EDGE ( 'NONE', *, *, #3725, .T. ) ;
#2065 = DIRECTION ( 'NONE',  ( -1.000000000000000000, -0.000000000000000000, -0.000000000000000000 ) ) ;
#2066 = EDGE_CURVE ( 'NONE', #4479, #398, #4900, .T. ) ;
#2067 = DIRECTION ( 'NONE',  ( -4.336808689942018722E-16, -1.000000000000000000, 0.000000000000000000 ) ) ;
#2068 = FACE_OUTER_BOUND ( 'NONE', #1782, .T. ) ;
#2069 = ORIENTED_EDGE ( 'NONE', *, *, #664, .T. ) ;
#2070 = ORIENTED_EDGE ( 'NONE', *, *, #1910, .F. ) ;
#2071 = CARTESIAN_POINT ( 'NONE',  ( 0.000000000000000000, 0.000000000000000000, -20.00000000000000000 ) ) ;
#2072 = PRODUCT_DEFINITION ( 'UNKNOWN', '', #3199, #485 ) ;
#2073 = CARTESIAN_POINT ( 'NONE',  ( 21.87894646962817902, 12.09631101282777621, -20.77489010396705638 ) ) ;
#2074 = EDGE_CURVE ( 'NONE', #398, #2990, #3445, .T. ) ;
#2075 = ORIENTED_EDGE ( 'NONE', *, *, #4563, .T. ) ;
#2076 = CYLINDRICAL_SURFACE ( 'NONE', #3040, 23.00000000000000711 ) ;
#2077 = ADVANCED_FACE ( 'NONE', ( #4954 ), #1372, .T. ) ;
#2078 = FACE_OUTER_BOUND ( 'NONE', #2443, .T. ) ;
#2079 = MANIFOLD_SOLID_BREP ( 'M5 Clearance Hole1', #4267 ) ;
#2080 = ORIENTED_EDGE ( 'NONE', *, *, #4705, .T. ) ;
#2081 = CIRCLE ( 'NONE', #4149, 2.099999999999997868 ) ;
#2082 = FACE_OUTER_BOUND ( 'NONE', #2337, .T. ) ;
#2083 = CARTESIAN_POINT ( 'NONE',  ( -25.00000000000000000, 3.061616997868383043E-15, -32.00000000000000000 ) ) ;
#2084 = FACE_OUTER_BOUND ( 'NONE', #1663, .T. ) ;
#2085 = ORIENTED_EDGE ( 'NONE', *, *, #4797, .F. ) ;
#2086 = VECTOR ( 'NONE', #1041, 1000.000000000000000 ) ;
#2087 = ORIENTED_EDGE ( 'NONE', *, *, #869, .T. ) ;
#2088 = DIRECTION ( 'NONE',  ( 0.000000000000000000, 0.000000000000000000, -1.000000000000000000 ) ) ;
#2089 = VECTOR ( 'NONE', #2785, 1000.000000000000000 ) ;
#2090 = CYLINDRICAL_SURFACE ( 'NONE', #3062, 2.649999999999992806 ) ;
#2091 = CARTESIAN_POINT ( 'NONE',  ( -7.216449660063538023E-15, 2.136559688479409280E-14, -12.00000000000000000 ) ) ;
#2092 = VERTEX_POINT ( 'NONE', #1466 ) ;
#2093 = ADVANCED_FACE ( 'NONE', ( #3874 ), #141, .F. ) ;
#2094 = CIRCLE ( 'NONE', #503, 1.000000000000000888 ) ;
#2095 = ORIENTED_EDGE ( 'NONE', *, *, #2502, .T. ) ;
#2096 = FILL_AREA_STYLE_COLOUR ( '', #4304 ) ;
#2097 = DIRECTION ( 'NONE',  ( 0.000000000000000000, 0.000000000000000000, -1.000000000000000000 ) ) ;
#2098 = CARTESIAN_POINT ( 'NONE',  ( 0.000000000000000000, 0.000000000000000000, 0.000000000000000000 ) ) ;
#2099 = DIRECTION ( 'NONE',  ( 1.000000000000000000, 0.000000000000000000, 0.000000000000000000 ) ) ;
#2100 = AXIS2_PLACEMENT_3D ( 'NONE', #2716, #4636, #79 ) ;
#2101 = ORIENTED_EDGE ( 'NONE', *, *, #2261, .F. ) ;
#2102 = EDGE_CURVE ( 'NONE', #894, #2727, #2758, .T. ) ;
#2103 = AXIS2_PLACEMENT_3D ( 'NONE', #2232, #2259, #1880 ) ;
#2104 = CIRCLE ( 'NONE', #975, 2.099999999999990763 ) ;
#2105 = DIRECTION ( 'NONE',  ( 0.000000000000000000, 0.000000000000000000, -1.000000000000000000 ) ) ;
#2106 = DIRECTION ( 'NONE',  ( 4.073394895316987600E-15, -1.000000000000000000, 0.000000000000000000 ) ) ;
#2107 = CIRCLE ( 'NONE', #2580, 2.041999999999999815 ) ;
#2108 = PRESENTATION_LAYER_ASSIGNMENT (  '', '', ( #3228 ) ) ;
#2109 = EDGE_LOOP ( 'NONE', ( #2650, #1660, #2686, #4663, #1090 ) ) ;
#2110 = EDGE_CURVE ( 'NONE', #2416, #4003, #4254, .T. ) ;
#2111 = ADVANCED_FACE ( 'NONE', ( #3200 ), #3129, .T. ) ;
#2112 = ADVANCED_FACE ( 'NONE', ( #3570 ), #3380, .T. ) ;
#2113 = AXIS2_PLACEMENT_3D ( 'NONE', #4128, #3800, #4584 ) ;
#2114 = CARTESIAN_POINT ( 'NONE',  ( -23.68543856465402797, 7.999999999999996447, -4.000000000000000000 ) ) ;
#2115 = APPLICATION_PROTOCOL_DEFINITION ( 'draft international standard', 'automotive_design', 1998, #1723 ) ;
#2116 = FILL_AREA_STYLE ('',( #1629 ) ) ;
#2117 = ORIENTED_EDGE ( 'NONE', *, *, #535, .F. ) ;
#2118 = CYLINDRICAL_SURFACE ( 'NONE', #3145, 2.500000000000000888 ) ;
#2119 = DIRECTION ( 'NONE',  ( -0.000000000000000000, -0.000000000000000000, 1.000000000000000000 ) ) ;
#2120 = DIRECTION ( 'NONE',  ( 1.000000000000000000, 0.000000000000000000, 0.000000000000000000 ) ) ;
#2121 = EDGE_LOOP ( 'NONE', ( #241, #4188, #2234, #1626, #4386, #1456 ) ) ;
#2122 = EDGE_LOOP ( 'NONE', ( #2299, #2127, #1808 ) ) ;
#2123 = DIRECTION ( 'NONE',  ( -2.036697447658493800E-15, 1.000000000000000000, 0.000000000000000000 ) ) ;
#2124 = CARTESIAN_POINT ( 'NONE',  ( -16.10609822396473945, -5.439999999999995062, -4.000000000000000000 ) ) ;
#2125 = VECTOR ( 'NONE', #175, 1000.000000000000114 ) ;
#2126 = DIRECTION ( 'NONE',  ( 1.000000000000000000, 0.000000000000000000, 0.000000000000000000 ) ) ;
#2127 = ORIENTED_EDGE ( 'NONE', *, *, #4045, .F. ) ;
#2128 = FACE_OUTER_BOUND ( 'NONE', #4827, .T. ) ;
#2129 = CARTESIAN_POINT ( 'NONE',  ( 0.000000000000000000, 11.10102051443364068, -32.00000000000000000 ) ) ;
#2130 = LINE ( 'NONE', #1365, #3134 ) ;
#2131 = EDGE_CURVE ( 'NONE', #1594, #2919, #1858, .T. ) ;
#2132 = ADVANCED_FACE ( 'NONE', ( #1223 ), #2399, .F. ) ;
#2133 = ORIENTED_EDGE ( 'NONE', *, *, #2624, .T. ) ;
#2134 = DIRECTION ( 'NONE',  ( 0.9474175425861609545, -0.3199999999999996181, 0.000000000000000000 ) ) ;
#2135 =( NAMED_UNIT ( * ) SI_UNIT ( $, .STERADIAN. ) SOLID_ANGLE_UNIT ( ) );
#2136 = CARTESIAN_POINT ( 'NONE',  ( 5.000000000000000888, 4.250000000000000000, 0.000000000000000000 ) ) ;
#2137 = EDGE_CURVE ( 'NONE', #1989, #45, #1196, .T. ) ;
#2138 = VERTEX_POINT ( 'NONE', #2375 ) ;
#2139 = DIRECTION ( 'NONE',  ( 0.000000000000000000, 0.000000000000000000, 1.000000000000000000 ) ) ;
#2140 = EDGE_CURVE ( 'NONE', #1912, #3903, #3472, .T. ) ;
#2141 = DIRECTION ( 'NONE',  ( 0.000000000000000000, 0.000000000000000000, -1.000000000000000000 ) ) ;
#2142 = DIRECTION ( 'NONE',  ( -1.000000000000000000, 0.000000000000000000, 0.000000000000000000 ) ) ;
#2143 = VERTEX_POINT ( 'NONE', #2832 ) ;
#2144 = ORIENTED_EDGE ( 'NONE', *, *, #234, .F. ) ;
#2145 = FACE_OUTER_BOUND ( 'NONE', #3876, .T. ) ;
#2146 = DIRECTION ( 'NONE',  ( 0.000000000000000000, 0.000000000000000000, -1.000000000000000000 ) ) ;
#2147 = LINE ( 'NONE', #1814, #3952 ) ;
#2148 =( GEOMETRIC_REPRESENTATION_CONTEXT ( 3 ) GLOBAL_UNCERTAINTY_ASSIGNED_CONTEXT ( ( #2386 ) ) GLOBAL_UNIT_ASSIGNED_CONTEXT ( ( #1732, #1356, #2520 ) ) REPRESENTATION_CONTEXT ( 'NONE', 'WORKASPACE' ) );
#2149 = ORIENTED_EDGE ( 'NONE', *, *, #1089, .F. ) ;
#2150 = CARTESIAN_POINT ( 'NONE',  ( -3.642919299551294898E-14, 16.00000000000000000, -26.00000000000000355 ) ) ;
#2151 = DIRECTION ( 'NONE',  ( 1.000000000000000000, -0.000000000000000000, -0.000000000000000000 ) ) ;
#2152 = CARTESIAN_POINT ( 'NONE',  ( 15.00000000000000000, -16.00000000000000000, -26.00000000000000355 ) ) ;
#2153 = APPLICATION_CONTEXT ( 'automotive_design' ) ;
#2154 = EDGE_LOOP ( 'NONE', ( #920, #1613, #2229, #4251, #1869, #4927 ) ) ;
#2155 = EDGE_CURVE ( 'NONE', #4219, #4279, #818, .T. ) ;
#2156 = DIRECTION ( 'NONE',  ( -1.000000000000000000, 0.000000000000000000, 0.000000000000000000 ) ) ;
#2157 = CARTESIAN_POINT ( 'NONE',  ( 0.2500000000000002220, 0.000000000000000000, 0.000000000000000000 ) ) ;
#2158 = ORIENTED_EDGE ( 'NONE', *, *, #4675, .F. ) ;
#2159 = CIRCLE ( 'NONE', #3749, 2.055000000000000160 ) ;
#2160 = ADVANCED_FACE ( 'NONE', ( #1665, #1642 ), #1618, .F. ) ;
#2161 = EDGE_CURVE ( 'NONE', #2782, #2138, #4694, .T. ) ;
#2162 = DIRECTION ( 'NONE',  ( 1.357798298438996130E-15, -1.000000000000000000, 0.000000000000000000 ) ) ;
#2163 = CARTESIAN_POINT ( 'NONE',  ( 0.000000000000000000, 0.000000000000000000, -32.00000000000000000 ) ) ;
#2164 = PRESENTATION_LAYER_ASSIGNMENT (  '', '', ( #4230 ) ) ;
#2165 = VERTEX_POINT ( 'NONE', #1947 ) ;
#2166 = ADVANCED_FACE ( 'NONE', ( #40 ), #4720, .T. ) ;
#2167 = EDGE_CURVE ( 'NONE', #1558, #4122, #1305, .T. ) ;
#2168 = VECTOR ( 'NONE', #4066, 1000.000000000000000 ) ;
#2169 = CARTESIAN_POINT ( 'NONE',  ( 0.000000000000000000, 0.000000000000000000, 2.000000000000001776 ) ) ;
#2170 = CARTESIAN_POINT ( 'NONE',  ( -21.37171027316247063, 8.500000000000072831, -4.000000000000000000 ) ) ;
#2171 = CARTESIAN_POINT ( 'NONE',  ( 22.03949535914419400, 11.80087472665740655, -21.71428571428571885 ) ) ;
#2172 = PLANE ( 'NONE',  #1314 ) ;
#2173 = ORIENTED_EDGE ( 'NONE', *, *, #1877, .T. ) ;
#2174 = CARTESIAN_POINT ( 'NONE',  ( 0.000000000000000000, 0.000000000000000000, -1.999999999999994893 ) ) ;
#2175 = CARTESIAN_POINT ( 'NONE',  ( -6.708203932499366751, -2.000000000000003553, -12.00000000000000000 ) ) ;
#2176 = VECTOR ( 'NONE', #195, 1000.000000000000114 ) ;
#2177 = DIRECTION ( 'NONE',  ( 1.000000000000000000, -0.000000000000000000, -0.000000000000000000 ) ) ;
#2178 = AXIS2_PLACEMENT_3D ( 'NONE', #757, #267, #3364 ) ;
#2179 = ORIENTED_EDGE ( 'NONE', *, *, #4409, .F. ) ;
#2180 = VECTOR ( 'NONE', #1260, 1000.000000000000000 ) ;
#2181 = VECTOR ( 'NONE', #2211, 1000.000000000000000 ) ;
#2182 = CARTESIAN_POINT ( 'NONE',  ( 0.000000000000000000, -1.178949249685213863, 2.042000000000002924 ) ) ;
#2183 = DIRECTION ( 'NONE',  ( 0.000000000000000000, 0.000000000000000000, -1.000000000000000000 ) ) ;
#2184 = ORIENTED_EDGE ( 'NONE', *, *, #2530, .F. ) ;
#2185 = VECTOR ( 'NONE', #4623, 1000.000000000000000 ) ;
#2186 = CIRCLE ( 'NONE', #2837, 1.535500000000000087 ) ;
#2187 = CARTESIAN_POINT ( 'NONE',  ( 22.65824501284922476, 10.56463292904780005, -23.45112747056584368 ) ) ;
#2188 = CARTESIAN_POINT ( 'NONE',  ( 8.500000000000003553, 21.37171027316251681, 12.00000000000000000 ) ) ;
#2189 = VECTOR ( 'NONE', #1066, 1000.000000000000000 ) ;
#2190 = CARTESIAN_POINT ( 'NONE',  ( 15.00000000000000178, 16.00000000000000000, -26.00000000000000355 ) ) ;
#2191 = ORIENTED_EDGE ( 'NONE', *, *, #3897, .F. ) ;
#2192 = AXIS2_PLACEMENT_3D ( 'NONE', #412, #1503, #4560 ) ;
#2193 = CARTESIAN_POINT ( 'NONE',  ( -8.500000000000000000, -21.37171027316251681, 4.000000000000000000 ) ) ;
#2194 = DIRECTION ( 'NONE',  ( 1.000000000000000000, -0.000000000000000000, -0.000000000000000000 ) ) ;
#2195 = ORIENTED_EDGE ( 'NONE', *, *, #2530, .T. ) ;
#2196 = DIRECTION ( 'NONE',  ( -1.000000000000000000, -0.000000000000000000, -0.000000000000000000 ) ) ;
#2197 = ADVANCED_FACE ( 'NONE', ( #923 ), #2724, .T. ) ;
#2198 = ORIENTED_EDGE ( 'NONE', *, *, #4051, .F. ) ;
#2199 = CIRCLE ( 'NONE', #498, 6.999999999999999112 ) ;
#2200 = CARTESIAN_POINT ( 'NONE',  ( -31.74999999999995737, 0.000000000000000000, 0.000000000000000000 ) ) ;
#2201 = CARTESIAN_POINT ( 'NONE',  ( 0.000000000000000000, 0.000000000000000000, 14.30577747056276472 ) ) ;
#2202 = STYLED_ITEM ( 'NONE', ( #2298 ), #425 ) ;
#2203 = CARTESIAN_POINT ( 'NONE',  ( 15.00000000000000000, -11.10102051443364424, -21.00000000000000000 ) ) ;
#2204 = EDGE_CURVE ( 'NONE', #2811, #2092, #268, .T. ) ;
#2205 = EDGE_CURVE ( 'NONE', #934, #4080, #4095, .T. ) ;
#2206 = VERTEX_POINT ( 'NONE', #4776 ) ;
#2207 = FACE_OUTER_BOUND ( 'NONE', #129, .T. ) ;
#2208 = CARTESIAN_POINT ( 'NONE',  ( -12.49999999999999822, -19.30673457630782863, 4.000000000000000000 ) ) ;
#2209 = DIRECTION ( 'NONE',  ( -0.000000000000000000, -0.000000000000000000, 1.000000000000000000 ) ) ;
#2210 = ORIENTED_EDGE ( 'NONE', *, *, #3343, .F. ) ;
#2211 = DIRECTION ( 'NONE',  ( -1.357798298438996130E-15, 1.000000000000000000, 0.000000000000000000 ) ) ;
#2212 = DIRECTION ( 'NONE',  ( 1.000000000000000000, 0.000000000000000000, 0.000000000000000000 ) ) ;
#2213 = DIRECTION ( 'NONE',  ( 1.000000000000000000, 0.000000000000000000, 0.000000000000000000 ) ) ;
#2214 = ORIENTED_EDGE ( 'NONE', *, *, #4204, .F. ) ;
#2215 = CARTESIAN_POINT ( 'NONE',  ( -9.000000000000001776, 2.000000000000000000, -32.00000000000000000 ) ) ;
#2216 = EDGE_CURVE ( 'NONE', #212, #4443, #2878, .T. ) ;
#2217 = DIRECTION ( 'NONE',  ( 0.000000000000000000, 0.000000000000000000, -1.000000000000000000 ) ) ;
#2218 = LINE ( 'NONE', #1831, #1295 ) ;
#2219 = PLANE ( 'NONE',  #2995 ) ;
#2220 = VERTEX_POINT ( 'NONE', #2897 ) ;
#2221 = CARTESIAN_POINT ( 'NONE',  ( 5.000000000000000888, 0.000000000000000000, 0.000000000000000000 ) ) ;
#2222 = PLANE ( 'NONE',  #4879 ) ;
#2223 = CARTESIAN_POINT ( 'NONE',  ( 0.000000000000000000, 0.000000000000000000, -4.000000000000000000 ) ) ;
#2224 = ORIENTED_EDGE ( 'NONE', *, *, #3717, .F. ) ;
#2225 = ADVANCED_FACE ( 'NONE', ( #3688 ), #4891, .F. ) ;
#2226 = CARTESIAN_POINT ( 'NONE',  ( 0.000000000000000000, 0.000000000000000000, -32.00000000000000000 ) ) ;
#2227 = DIRECTION ( 'NONE',  ( 0.000000000000000000, 0.8660254037844380415, -0.5000000000000012212 ) ) ;
#2228 = CARTESIAN_POINT ( 'NONE',  ( 0.000000000000000000, 0.000000000000000000, -4.000000000000000000 ) ) ;
#2229 = ORIENTED_EDGE ( 'NONE', *, *, #1574, .T. ) ;
#2230 = DIRECTION ( 'NONE',  ( -0.000000000000000000, 0.8660254037844391517, 0.4999999999999990563 ) ) ;
#2231 = CARTESIAN_POINT ( 'NONE',  ( -9.000000000000001776, 2.000000000000000000, -32.00000000000000000 ) ) ;
#2232 = CARTESIAN_POINT ( 'NONE',  ( 3.999999999999999112, 3.500000000000000000, 0.000000000000000000 ) ) ;
#2233 = ORIENTED_EDGE ( 'NONE', *, *, #4390, .T. ) ;
#2234 = ORIENTED_EDGE ( 'NONE', *, *, #601, .F. ) ;
#2235 = DIRECTION ( 'NONE',  ( -1.284618353679617394E-16, 3.717779911235453901E-17, 1.000000000000000000 ) ) ;
#2236 = AXIS2_PLACEMENT_3D ( 'NONE', #3594, #897, #3974 ) ;
#2237 = DIRECTION ( 'NONE',  ( 0.000000000000000000, 0.000000000000000000, 1.000000000000000000 ) ) ;
#2238 = CARTESIAN_POINT ( 'NONE',  ( 2.500000000000000000, 2.357898499370433054, -1.951563910473907981E-15 ) ) ;
#2239 = CARTESIAN_POINT ( 'NONE',  ( 15.00000000000000000, 20.00000000000000355, -20.00000000000000000 ) ) ;
#2240 = VERTEX_POINT ( 'NONE', #943 ) ;
#2241 = LINE ( 'NONE', #2948, #3938 ) ;
#2242 = SURFACE_STYLE_USAGE ( .BOTH. , #4191 ) ;
#2243 = DIRECTION ( 'NONE',  ( -0.000000000000000000, -0.000000000000000000, -1.000000000000000000 ) ) ;
#2244 =( NAMED_UNIT ( * ) PLANE_ANGLE_UNIT ( ) SI_UNIT ( $, .RADIAN. ) );
#2245 = CIRCLE ( 'NONE', #3674, 1.535500000000000087 ) ;
#2246 = EDGE_LOOP ( 'NONE', ( #693, #3010, #1096, #4701, #563, #4382 ) ) ;
#2247 = AXIS2_PLACEMENT_3D ( 'NONE', #4120, #4953, #691 ) ;
#2248 = UNCERTAINTY_MEASURE_WITH_UNIT (LENGTH_MEASURE( 1.000000000000000082E-05 ), #695, 'distance_accuracy_value', 'NONE');
#2249 = DIRECTION ( 'NONE',  ( 0.000000000000000000, 0.000000000000000000, -1.000000000000000000 ) ) ;
#2250 = FACE_OUTER_BOUND ( 'NONE', #3428, .T. ) ;
#2251 = AXIS2_PLACEMENT_3D ( 'NONE', #704, #3760, #1428 ) ;
#2252 = ADVANCED_FACE ( 'NONE', ( #3992 ), #1408, .T. ) ;
#2253 = EDGE_CURVE ( 'NONE', #240, #3209, #1388, .T. ) ;
#2254 = EDGE_LOOP ( 'NONE', ( #2849, #274, #1410, #2600 ) ) ;
#2255 = AXIS2_PLACEMENT_3D ( 'NONE', #700, #3387, #2963 ) ;
#2256 = VECTOR ( 'NONE', #304, 1000.000000000000000 ) ;
#2257 = CARTESIAN_POINT ( 'NONE',  ( 25.00000000000000000, 16.00000000000000000, -26.00000000000000355 ) ) ;
#2258 = FACE_OUTER_BOUND ( 'NONE', #1672, .T. ) ;
#2259 = DIRECTION ( 'NONE',  ( 1.000000000000000000, 0.000000000000000000, 0.000000000000000000 ) ) ;
#2260 = CARTESIAN_POINT ( 'NONE',  ( -6.517431832507181422E-14, 16.00000000000000000, -26.00000000000000355 ) ) ;
#2261 = EDGE_CURVE ( 'NONE', #4758, #4052, #1012, .T. ) ;
#2262 = AXIS2_PLACEMENT_3D ( 'NONE', #3150, #522, #1636 ) ;
#2263 = ORIENTED_EDGE ( 'NONE', *, *, #3355, .F. ) ;
#2264 =( GEOMETRIC_REPRESENTATION_CONTEXT ( 3 ) GLOBAL_UNCERTAINTY_ASSIGNED_CONTEXT ( ( #4545 ) ) GLOBAL_UNIT_ASSIGNED_CONTEXT ( ( #976, #3281, #1004 ) ) REPRESENTATION_CONTEXT ( 'NONE', 'WORKASPACE' ) );
#2265 = DIRECTION ( 'NONE',  ( -0.000000000000000000, -0.000000000000000000, 1.000000000000000000 ) ) ;
#2266 = CARTESIAN_POINT ( 'NONE',  ( -10.00000000000002132, 16.00000000000000000, -26.00000000000000355 ) ) ;
#2267 = LINE ( 'NONE', #1140, #1547 ) ;
#2268 = ORIENTED_EDGE ( 'NONE', *, *, #1447, .T. ) ;
#2269 = CARTESIAN_POINT ( 'NONE',  ( 2.444036937190193033E-14, 6.999999999999999112, -32.00000000000000000 ) ) ;
#2270 = EDGE_CURVE ( 'NONE', #4747, #406, #2923, .T. ) ;
#2271 = CARTESIAN_POINT ( 'NONE',  ( -2.172477277502393807E-14, 16.00000000000000000, -23.90000000000000924 ) ) ;
#2272 = CLOSED_SHELL ( 'NONE', ( #999, #783, #1662, #71, #1746, #3505, #3879, #2459, #3204, #4444, #3625, #2166, #3583, #220, #3529, #2962, #120, #2077, #70, #387, #2957, #355, #3652, #494, #47, #998, #2851 ) ) ;
#2273 = VERTEX_POINT ( 'NONE', #2124 ) ;
#2274 = AXIS2_PLACEMENT_3D ( 'NONE', #3074, #3168, #2310 ) ;
#2275 = FACE_OUTER_BOUND ( 'NONE', #1038, .T. ) ;
#2276 = EDGE_CURVE ( 'NONE', #3321, #4346, #3639, .T. ) ;
#2277 = DIRECTION ( 'NONE',  ( 0.000000000000000000, 0.000000000000000000, -1.000000000000000000 ) ) ;
#2278 = EDGE_CURVE ( 'NONE', #1461, #1716, #1309, .T. ) ;
#2279 = ORIENTED_EDGE ( 'NONE', *, *, #3940, .T. ) ;
#2280 = ADVANCED_FACE ( 'NONE', ( #1322 ), #4414, .F. ) ;
#2281 = CARTESIAN_POINT ( 'NONE',  ( 22.82279522939548144, 10.20431389251127463, -27.60486197633221650 ) ) ;
#2282 = FACE_OUTER_BOUND ( 'NONE', #1238, .T. ) ;
#2283 = CARTESIAN_POINT ( 'NONE',  ( 19.30673457630784995, 12.49999999999993783, -4.000000000000000000 ) ) ;
#2284 = DIRECTION ( 'NONE',  ( 1.000000000000000000, 0.000000000000000000, -0.000000000000000000 ) ) ;
#2285 = ORIENTED_EDGE ( 'NONE', *, *, #2412, .F. ) ;
#2286 = EDGE_CURVE ( 'NONE', #4866, #3891, #298, .T. ) ;
#2287 = CARTESIAN_POINT ( 'NONE',  ( 0.000000000000000000, -1.999999999999999112, -20.00000000000000000 ) ) ;
#2288 = FILL_AREA_STYLE ('',( #4844 ) ) ;
#2289 = CARTESIAN_POINT ( 'NONE',  ( 2.000000000000000000, 1.773042676681340968, -2.276824562219559311E-15 ) ) ;
#2290 = CARTESIAN_POINT ( 'NONE',  ( -9.000000000000003553, -1.999999999999999112, -20.00000000000000000 ) ) ;
#2291 = CARTESIAN_POINT ( 'NONE',  ( 22.35373982437574014, 11.19469724424307167, -32.00000000000000711 ) ) ;
#2292 = ORIENTED_EDGE ( 'NONE', *, *, #3572, .T. ) ;
#2293 = ORIENTED_EDGE ( 'NONE', *, *, #4030, .T. ) ;
#2294 = DIRECTION ( 'NONE',  ( 0.000000000000000000, 0.000000000000000000, -1.000000000000000000 ) ) ;
#2295 = FILL_AREA_STYLE ('',( #4599 ) ) ;
#2296 = ORIENTED_EDGE ( 'NONE', *, *, #462, .T. ) ;
#2297 = DIRECTION ( 'NONE',  ( -1.000000000000000000, -0.000000000000000000, -0.000000000000000000 ) ) ;
#2298 = PRESENTATION_STYLE_ASSIGNMENT (( #4935 ) ) ;
#2299 = ORIENTED_EDGE ( 'NONE', *, *, #3113, .F. ) ;
#2300 = ORIENTED_EDGE ( 'NONE', *, *, #2651, .T. ) ;
#2301 = CARTESIAN_POINT ( 'NONE',  ( -31.74999999999995737, 0.000000000000000000, 0.000000000000000000 ) ) ;
#2302 = LINE ( 'NONE', #3751, #1857 ) ;
#2303 = DIRECTION ( 'NONE',  ( -0.7071067811865469066, 0.000000000000000000, -0.7071067811865482389 ) ) ;
#2304 = LINE ( 'NONE', #3826, #2028 ) ;
#2305 = EDGE_CURVE ( 'NONE', #2020, #991, #269, .T. ) ;
#2306 =( REPRESENTATION_RELATIONSHIP ('NONE','NONE', #137, #3720 ) REPRESENTATION_RELATIONSHIP_WITH_TRANSFORMATION ( #3745 )SHAPE_REPRESENTATION_RELATIONSHIP( ) );
#2307 = PRODUCT_DEFINITION ( 'UNKNOWN', '', #3822, #1978 ) ;
#2308 = ORIENTED_EDGE ( 'NONE', *, *, #4024, .T. ) ;
#2309 = EDGE_CURVE ( 'NONE', #4716, #536, #4752, .T. ) ;
#2310 = DIRECTION ( 'NONE',  ( 1.000000000000000000, 0.000000000000000000, 0.000000000000000000 ) ) ;
#2311 =( NAMED_UNIT ( * ) SI_UNIT ( $, .STERADIAN. ) SOLID_ANGLE_UNIT ( ) );
#2312 = CARTESIAN_POINT ( 'NONE',  ( 2.000000000000000000, -1.502314598737159623E-15, -1.535500000000000087 ) ) ;
#2313 = LINE ( 'NONE', #111, #1763 ) ;
#2314 = CARTESIAN_POINT ( 'NONE',  ( 21.90226041726126383, -12.05376714070079025, -20.67955005196816032 ) ) ;
#2315 = EDGE_CURVE ( 'NONE', #1031, #4739, #171, .T. ) ;
#2316 = EDGE_CURVE ( 'NONE', #148, #597, #2860, .T. ) ;
#2317 = ORIENTED_EDGE ( 'NONE', *, *, #2412, .T. ) ;
#2318 = CIRCLE ( 'NONE', #793, 22.99999999999998934 ) ;
#2319 = ORIENTED_EDGE ( 'NONE', *, *, #4172, .T. ) ;
#2320 =( NAMED_UNIT ( * ) SI_UNIT ( $, .STERADIAN. ) SOLID_ANGLE_UNIT ( ) );
#2321 = DIRECTION ( 'NONE',  ( -1.000000000000000000, -0.000000000000000000, -0.000000000000000000 ) ) ;
#2322 = SURFACE_STYLE_FILL_AREA ( #787 ) ;
#2323 = DIRECTION ( 'NONE',  ( 0.000000000000000000, -0.5000000000000011102, -0.8660254037844379305 ) ) ;
#2324 = AXIS2_PLACEMENT_3D ( 'NONE', #3007, #2949, #3275 ) ;
#2325 = ORIENTED_EDGE ( 'NONE', *, *, #2066, .F. ) ;
#2326 = CARTESIAN_POINT ( 'NONE',  ( 0.000000000000000000, 0.000000000000000000, -12.00000000000000000 ) ) ;
#2327 = CARTESIAN_POINT ( 'NONE',  ( 4.199999999999995737, 0.000000000000000000, 0.000000000000000000 ) ) ;
#2328 = CIRCLE ( 'NONE', #639, 23.00000000000000711 ) ;
#2329 = ORIENTED_EDGE ( 'NONE', *, *, #2349, .T. ) ;
#2330 = ORIENTED_EDGE ( 'NONE', *, *, #2216, .T. ) ;
#2331 = VECTOR ( 'NONE', #2950, 1000.000000000000000 ) ;
#2332 = UNCERTAINTY_MEASURE_WITH_UNIT (LENGTH_MEASURE( 1.000000000000000082E-05 ), #1386, 'distance_accuracy_value', 'NONE');
#2333 = VECTOR ( 'NONE', #4016, 1000.000000000000000 ) ;
#2334 = DIRECTION ( 'NONE',  ( 0.000000000000000000, 0.000000000000000000, -1.000000000000000000 ) ) ;
#2335 = CARTESIAN_POINT ( 'NONE',  ( 2.500000000000000000, -1.178949249685213863, 2.042000000000002924 ) ) ;
#2336 = FACE_OUTER_BOUND ( 'NONE', #2713, .T. ) ;
#2337 = EDGE_LOOP ( 'NONE', ( #1198, #1977, #3574, #2996 ) ) ;
#2338 = ORIENTED_EDGE ( 'NONE', *, *, #690, .T. ) ;
#2339 = AXIS2_PLACEMENT_3D ( 'NONE', #3825, #2365, #3140 ) ;
#2340 = CARTESIAN_POINT ( 'NONE',  ( 0.000000000000000000, -0.8865213383406721492, -1.535499999999999199 ) ) ;
#2341 = CARTESIAN_POINT ( 'NONE',  ( 6.999999999999999112, 0.000000000000000000, -32.00000000000000000 ) ) ;
#2342 = VECTOR ( 'NONE', #3419, 1000.000000000000000 ) ;
#2343 = AXIS2_PLACEMENT_3D ( 'NONE', #2260, #378, #3802 ) ;
#2344 = AXIS2_PLACEMENT_3D ( 'NONE', #3895, #3550, #2430 ) ;
#2345 = VERTEX_POINT ( 'NONE', #4532 ) ;
#2346 = CIRCLE ( 'NONE', #983, 25.00000000000000000 ) ;
#2347 = ORIENTED_EDGE ( 'NONE', *, *, #4768, .F. ) ;
#2348 = SURFACE_SIDE_STYLE ('',( #4930 ) ) ;
#2349 = EDGE_CURVE ( 'NONE', #4716, #3536, #253, .T. ) ;
#2350 = CARTESIAN_POINT ( 'NONE',  ( 0.1999999999999987899, 0.000000000000000000, 0.000000000000000000 ) ) ;
#2351 = EDGE_CURVE ( 'NONE', #2431, #3852, #4869, .T. ) ;
#2352 = DIRECTION ( 'NONE',  ( 0.000000000000000000, 0.000000000000000000, -1.000000000000000000 ) ) ;
#2353 = DIRECTION ( 'NONE',  ( -1.000000000000000000, 0.000000000000000000, 0.000000000000000000 ) ) ;
#2354 = VECTOR ( 'NONE', #3273, 1000.000000000000000 ) ;
#2355 = ORIENTED_EDGE ( 'NONE', *, *, #1187, .F. ) ;
#2356 = UNCERTAINTY_MEASURE_WITH_UNIT (LENGTH_MEASURE( 1.000000000000000082E-05 ), #630, 'distance_accuracy_value', 'NONE');
#2357 = DIRECTION ( 'NONE',  ( 1.000000000000000000, 0.000000000000000000, 0.000000000000000000 ) ) ;
#2358 = ADVANCED_FACE ( 'NONE', ( #1087 ), #2619, .T. ) ;
#2359 = LINE ( 'NONE', #4277, #1435 ) ;
#2360 = ORIENTED_EDGE ( 'NONE', *, *, #4767, .F. ) ;
#2361 = ORIENTED_EDGE ( 'NONE', *, *, #4579, .T. ) ;
#2362 = CIRCLE ( 'NONE', #4759, 6.999999999999999112 ) ;
#2363 = CARTESIAN_POINT ( 'NONE',  ( 22.91733123609770928, -9.989778454058074075, -26.00578286613768597 ) ) ;
#2364 = CARTESIAN_POINT ( 'NONE',  ( 15.00000000000000000, -11.10102051443364424, -20.00000000000000000 ) ) ;
#2365 = DIRECTION ( 'NONE',  ( 1.000000000000000000, 0.000000000000000000, 0.000000000000000000 ) ) ;
#2366 = VERTEX_POINT ( 'NONE', #3393 ) ;
#2367 = ORIENTED_EDGE ( 'NONE', *, *, #1154, .T. ) ;
#2368 = ITEM_DEFINED_TRANSFORMATION ( 'NONE', 'NONE', #3114,  #1918 ) ;
#2369 = DIRECTION ( 'NONE',  ( 0.000000000000000000, 0.000000000000000000, -1.000000000000000000 ) ) ;
#2370 = DIRECTION ( 'NONE',  ( 0.000000000000000000, -1.000000000000000000, 0.000000000000000000 ) ) ;
#2371 = FACE_OUTER_BOUND ( 'NONE', #3969, .T. ) ;
#2372 = EDGE_LOOP ( 'NONE', ( #549, #473, #3545, #1272, #4448 ) ) ;
#2373 = ORIENTED_EDGE ( 'NONE', *, *, #3996, .F. ) ;
#2374 = CARTESIAN_POINT ( 'NONE',  ( -31.74999999999995737, 0.000000000000000000, 2.000000000000000888 ) ) ;
#2375 = CARTESIAN_POINT ( 'NONE',  ( 0.000000000000000000, -25.00000000000000000, -20.00000000000000000 ) ) ;
#2376 = CARTESIAN_POINT ( 'NONE',  ( 15.00000000000000178, 16.00000000000000000, -28.64999999999998792 ) ) ;
#2377 = EDGE_LOOP ( 'NONE', ( #114, #3510 ) ) ;
#2378 = EDGE_CURVE ( 'NONE', #1707, #2498, #3735, .T. ) ;
#2379 = EDGE_CURVE ( 'NONE', #3315, #484, #4100, .T. ) ;
#2380 = DIRECTION ( 'NONE',  ( -1.000000000000000000, 0.000000000000000000, 0.000000000000000000 ) ) ;
#2381 = CARTESIAN_POINT ( 'NONE',  ( 0.000000000000000000, -11.10102051443364068, -32.00000000000000000 ) ) ;
#2382 = ORIENTED_EDGE ( 'NONE', *, *, #4563, .F. ) ;
#2383 = EDGE_LOOP ( 'NONE', ( #1078, #3581, #2059 ) ) ;
#2384 = ADVANCED_FACE ( 'NONE', ( #660 ), #4949, .F. ) ;
#2385 = EDGE_CURVE ( 'NONE', #4859, #2525, #1862, .T. ) ;
#2386 = UNCERTAINTY_MEASURE_WITH_UNIT (LENGTH_MEASURE( 1.000000000000000082E-05 ), #1732, 'distance_accuracy_value', 'NONE');
#2387 = DIRECTION ( 'NONE',  ( 0.000000000000000000, 0.000000000000000000, 1.000000000000000000 ) ) ;
#2388 = CARTESIAN_POINT ( 'NONE',  ( 15.00000000000000000, -16.00000000000000000, -26.00000000000000355 ) ) ;
#2389 = ORIENTED_EDGE ( 'NONE', *, *, #2351, .T. ) ;
#2390 = ORIENTED_EDGE ( 'NONE', *, *, #1673, .F. ) ;
#2391 =( NAMED_UNIT ( * ) PLANE_ANGLE_UNIT ( ) SI_UNIT ( $, .RADIAN. ) );
#2392 = CARTESIAN_POINT ( 'NONE',  ( -3.666055405785289392E-14, -6.999999999999999112, -20.00000000000000000 ) ) ;
#2393 = CARTESIAN_POINT ( 'NONE',  ( 0.2500000000000002220, 0.000000000000000000, 0.000000000000000000 ) ) ;
#2394 = AXIS2_PLACEMENT_3D ( 'NONE', #4614, #1085, #1529 ) ;
#2395 = ORIENTED_EDGE ( 'NONE', *, *, #4298, .F. ) ;
#2396 = VERTEX_POINT ( 'NONE', #336 ) ;
#2397 = FILL_AREA_STYLE_COLOUR ( '', #1188 ) ;
#2398 = LINE ( 'NONE', #2051, #4399 ) ;
#2399 = CYLINDRICAL_SURFACE ( 'NONE', #1227, 2.099999999999997868 ) ;
#2400 = EDGE_CURVE ( 'NONE', #1400, #2525, #4087, .T. ) ;
#2401 = CARTESIAN_POINT ( 'NONE',  ( 0.000000000000000000, 0.000000000000000000, -4.000000000000000000 ) ) ;
#2402 = ORIENTED_EDGE ( 'NONE', *, *, #963, .T. ) ;
#2403 = CARTESIAN_POINT ( 'NONE',  ( -8.500000000000003553, 21.37171027316251681, 12.00000000000000000 ) ) ;
#2404 = LINE ( 'NONE', #2807, #4396 ) ;
#2405 = AXIS2_PLACEMENT_3D ( 'NONE', #4102, #618, #3726 ) ;
#2406 = ORIENTED_EDGE ( 'NONE', *, *, #3705, .F. ) ;
#2407 = ORIENTED_EDGE ( 'NONE', *, *, #3872, .F. ) ;
#2408 = VECTOR ( 'NONE', #1867, 1000.000000000000000 ) ;
#2409 = CARTESIAN_POINT ( 'NONE',  ( -31.74999999999995737, 0.000000000000000000, 0.000000000000000000 ) ) ;
#2410 = DIRECTION ( 'NONE',  ( 0.000000000000000000, 0.000000000000000000, -1.000000000000000000 ) ) ;
#2411 = FACE_BOUND ( 'NONE', #3917, .T. ) ;
#2412 = EDGE_CURVE ( 'NONE', #4052, #1430, #3024, .T. ) ;
#2413 = LINE ( 'NONE', #3431, #3224 ) ;
#2414 = VECTOR ( 'NONE', #922, 1000.000000000000000 ) ;
#2415 = ORIENTED_EDGE ( 'NONE', *, *, #2349, .F. ) ;
#2416 = VERTEX_POINT ( 'NONE', #4510 ) ;
#2417 = AXIS2_PLACEMENT_3D ( 'NONE', #1786, #546, #1690 ) ;
#2418 = AXIS2_PLACEMENT_3D ( 'NONE', #3271, #4719, #608 ) ;
#2419 = DIRECTION ( 'NONE',  ( 0.000000000000000000, 0.000000000000000000, 1.000000000000000000 ) ) ;
#2420 = DIRECTION ( 'NONE',  ( 1.000000000000000000, -0.000000000000000000, -0.000000000000000000 ) ) ;
#2421 = CYLINDRICAL_SURFACE ( 'NONE', #1700, 1.000000000000000888 ) ;
#2422 = AXIS2_PLACEMENT_3D ( 'NONE', #1160, #2690, #4201 ) ;
#2423 = VECTOR ( 'NONE', #310, 1000.000000000000000 ) ;
#2424 = ORIENTED_EDGE ( 'NONE', *, *, #870, .F. ) ;
#2425 = ORIENTED_EDGE ( 'NONE', *, *, #272, .T. ) ;
#2426 = AXIS2_PLACEMENT_3D ( 'NONE', #4042, #144, #4373 ) ;
#2427 = VECTOR ( 'NONE', #561, 1000.000000000000000 ) ;
#2428 = PLANE ( 'NONE',  #1686 ) ;
#2429 = CIRCLE ( 'NONE', #3066, 25.00000000000000000 ) ;
#2430 = DIRECTION ( 'NONE',  ( 0.000000000000000000, 0.000000000000000000, -1.000000000000000000 ) ) ;
#2431 = VERTEX_POINT ( 'NONE', #2971 ) ;
#2432 = AXIS2_PLACEMENT_3D ( 'NONE', #4240, #454, #1589 ) ;
#2433 = DIRECTION ( 'NONE',  ( -0.000000000000000000, -0.000000000000000000, 1.000000000000000000 ) ) ;
#2434 = CARTESIAN_POINT ( 'NONE',  ( 0.000000000000000000, 0.000000000000000000, -20.00000000000000000 ) ) ;
#2435 = AXIS2_PLACEMENT_3D ( 'NONE', #4940, #2663, #2458 ) ;
#2436 = ORIENTED_EDGE ( 'NONE', *, *, #1839, .F. ) ;
#2437 = EDGE_CURVE ( 'NONE', #4655, #4738, #2639, .T. ) ;
#2438 = ADVANCED_FACE ( 'NONE', ( #3808 ), #1127, .F. ) ;
#2439 = PLANE ( 'NONE',  #2681 ) ;
#2440 = FILL_AREA_STYLE_COLOUR ( '', #3300 ) ;
#2441 = CARTESIAN_POINT ( 'NONE',  ( 2.500000000000000000, 2.357898499370433054, -1.951563910473907981E-15 ) ) ;
#2442 = ORIENTED_EDGE ( 'NONE', *, *, #2309, .F. ) ;
#2443 = EDGE_LOOP ( 'NONE', ( #3923, #1646, #847, #3769 ) ) ;
#2444 = CIRCLE ( 'NONE', #3479, 25.00000000000000000 ) ;
#2445 = DIRECTION ( 'NONE',  ( 0.000000000000000000, 0.000000000000000000, 1.000000000000000000 ) ) ;
#2446 = DIRECTION ( 'NONE',  ( -0.000000000000000000, 0.000000000000000000, 1.000000000000000000 ) ) ;
#2447 = CARTESIAN_POINT ( 'NONE',  ( 24.00000000000000000, 1.610000000000000098, 0.000000000000000000 ) ) ;
#2448 = ORIENTED_EDGE ( 'NONE', *, *, #930, .F. ) ;
#2449 = ADVANCED_FACE ( 'NONE', ( #4559 ), #1887, .F. ) ;
#2450 = ORIENTED_EDGE ( 'NONE', *, *, #3269, .T. ) ;
#2451 = CARTESIAN_POINT ( 'NONE',  ( 3.999999999999999112, 0.000000000000000000, 0.000000000000000000 ) ) ;
#2452 = DIRECTION ( 'NONE',  ( 1.106769389831504682E-16, -1.000000000000000000, 0.000000000000000000 ) ) ;
#2453 = ORIENTED_EDGE ( 'NONE', *, *, #1385, .F. ) ;
#2454 = DIRECTION ( 'NONE',  ( -1.000000000000000000, -0.000000000000000000, -0.000000000000000000 ) ) ;
#2455 = CARTESIAN_POINT ( 'NONE',  ( 19.30673457630776468, -12.50000000000007105, -4.000000000000000000 ) ) ;
#2456 = VERTEX_POINT ( 'NONE', #4483 ) ;
#2457 = CARTESIAN_POINT ( 'NONE',  ( -23.68543856465402442, -8.000000000000003553, -4.000000000000000000 ) ) ;
#2458 = DIRECTION ( 'NONE',  ( -1.000000000000000000, 0.000000000000000000, 0.000000000000000000 ) ) ;
#2459 = ADVANCED_FACE ( 'NONE', ( #365 ), #290, .T. ) ;
#2460 = ORIENTED_EDGE ( 'NONE', *, *, #2010, .T. ) ;
#2461 = ORIENTED_EDGE ( 'NONE', *, *, #4083, .F. ) ;
#2462 = DIRECTION ( 'NONE',  ( -1.000000000000000000, 0.000000000000000000, 0.000000000000000000 ) ) ;
#2463 = CARTESIAN_POINT ( 'NONE',  ( 4.196500603111122875E-14, 12.50000000000000178, -12.00000000000000000 ) ) ;
#2464 = CARTESIAN_POINT ( 'NONE',  ( 21.96462198364264395, -11.94070939570634948, -21.57727627927737046 ) ) ;
#2465 = ADVANCED_FACE ( 'NONE', ( #4186 ), #758, .F. ) ;
#2466 = ORIENTED_EDGE ( 'NONE', *, *, #1602, .F. ) ;
#2467 = ORIENTED_EDGE ( 'NONE', *, *, #3705, .T. ) ;
#2468 =( NAMED_UNIT ( * ) PLANE_ANGLE_UNIT ( ) SI_UNIT ( $, .RADIAN. ) );
#2469 = DIRECTION ( 'NONE',  ( 1.000000000000000000, -0.000000000000000000, -0.000000000000000000 ) ) ;
#2470 = DIRECTION ( 'NONE',  ( -0.000000000000000000, -0.000000000000000000, 1.000000000000000000 ) ) ;
#2471 = CARTESIAN_POINT ( 'NONE',  ( 0.000000000000000000, 0.000000000000000000, 12.00000000000000000 ) ) ;
#2472 = EDGE_CURVE ( 'NONE', #3165, #1024, #2495, .T. ) ;
#2473 = EDGE_CURVE ( 'NONE', #1518, #4266, #2218, .T. ) ;
#2474 = ORIENTED_EDGE ( 'NONE', *, *, #1249, .F. ) ;
#2475 = DIRECTION ( 'NONE',  ( 1.000000000000000000, -0.000000000000000000, -0.000000000000000000 ) ) ;
#2476 = CARTESIAN_POINT ( 'NONE',  ( 16.10609822396473589, 5.440000000000003055, -12.00000000000000000 ) ) ;
#2477 = CARTESIAN_POINT ( 'NONE',  ( 25.00000000000000000, 0.000000000000000000, -32.00000000000000000 ) ) ;
#2478 = ORIENTED_EDGE ( 'NONE', *, *, #4572, .F. ) ;
#2479 = VECTOR ( 'NONE', #43, 1000.000000000000000 ) ;
#2480 = CARTESIAN_POINT ( 'NONE',  ( 0.000000000000000000, 0.000000000000000000, -32.00000000000000000 ) ) ;
#2481 = SHAPE_DEFINITION_REPRESENTATION ( #4819, #1326 ) ;
#2482 = CARTESIAN_POINT ( 'NONE',  ( 2.500000000000000000, -1.768423874527823569, 1.021000000000002794 ) ) ;
#2483 = CARTESIAN_POINT ( 'NONE',  ( 0.000000000000000000, -1.999999999999999112, -12.00000000000000000 ) ) ;
#2484 = ORIENTED_EDGE ( 'NONE', *, *, #53, .F. ) ;
#2485 = CIRCLE ( 'NONE', #4962, 25.00000000000000000 ) ;
#2486 = CARTESIAN_POINT ( 'NONE',  ( -16.10609822396473589, 5.440000000000003055, 14.30577747056276472 ) ) ;
#2487 = CARTESIAN_POINT ( 'NONE',  ( 0.000000000000000000, 0.000000000000000000, -20.00000000000000000 ) ) ;
#2488 = DIRECTION ( 'NONE',  ( -0.000000000000000000, 0.000000000000000000, 1.000000000000000000 ) ) ;
#2489 = ORIENTED_EDGE ( 'NONE', *, *, #4160, .T. ) ;
#2490 = AXIS2_PLACEMENT_3D ( 'NONE', #453, #3471, #86 ) ;
#2491 = VERTEX_POINT ( 'NONE', #4637 ) ;
#2492 = EDGE_CURVE ( 'NONE', #4739, #4372, #495, .T. ) ;
#2493 = CARTESIAN_POINT ( 'NONE',  ( 0.000000000000000000, -1.773042676681340968, 2.059984127722458425E-15 ) ) ;
#2494 = DIRECTION ( 'NONE',  ( -1.000000000000000000, 0.000000000000000000, 0.000000000000000000 ) ) ;
#2495 = CIRCLE ( 'NONE', #3448, 25.00000000000000000 ) ;
#2496 = ORIENTED_EDGE ( 'NONE', *, *, #288, .T. ) ;
#2497 = VECTOR ( 'NONE', #110, 1000.000000000000114 ) ;
#2498 = VERTEX_POINT ( 'NONE', #1243 ) ;
#2499 = CIRCLE ( 'NONE', #2422, 2.099999999999990763 ) ;
#2500 = CIRCLE ( 'NONE', #339, 0.2500000000000002220 ) ;
#2501 = CARTESIAN_POINT ( 'NONE',  ( 2.302289838212012812E-14, -16.00000000000000000, -26.00000000000000355 ) ) ;
#2502 = EDGE_CURVE ( 'NONE', #1283, #4080, #1048, .T. ) ;
#2503 = CARTESIAN_POINT ( 'NONE',  ( 24.55500000000002103, 0.000000000000000000, 0.000000000000000000 ) ) ;
#2504 = LINE ( 'NONE', #551, #720 ) ;
#2505 = AXIS2_PLACEMENT_3D ( 'NONE', #4684, #2792, #4764 ) ;
#2506 = AXIS2_PLACEMENT_3D ( 'NONE', #4, #1215, #4159 ) ;
#2507 = VECTOR ( 'NONE', #3159, 1000.000000000000000 ) ;
#2508 = ORIENTED_EDGE ( 'NONE', *, *, #4204, .T. ) ;
#2509 = EDGE_CURVE ( 'NONE', #654, #2138, #3564, .T. ) ;
#2510 = CONICAL_SURFACE ( 'NONE', #583, 2.099999999999997868, 1.029744258676653423 ) ;
#2511 = DIRECTION ( 'NONE',  ( 0.000000000000000000, 0.000000000000000000, 1.000000000000000000 ) ) ;
#2512 = DIRECTION ( 'NONE',  ( 1.000000000000000000, -0.000000000000000000, -0.000000000000000000 ) ) ;
#2513 = CYLINDRICAL_SURFACE ( 'NONE', #4816, 22.99999999999998934 ) ;
#2514 = ORIENTED_EDGE ( 'NONE', *, *, #489, .F. ) ;
#2515 = DIRECTION ( 'NONE',  ( -1.000000000000000000, 0.000000000000000000, -0.000000000000000000 ) ) ;
#2516 = CARTESIAN_POINT ( 'NONE',  ( 0.000000000000000000, 1.178949249685218525, 2.041999999999999371 ) ) ;
#2517 = FACE_OUTER_BOUND ( 'NONE', #4110, .T. ) ;
#2518 = ORIENTED_EDGE ( 'NONE', *, *, #1051, .T. ) ;
#2519 = EDGE_LOOP ( 'NONE', ( #3526, #283, #3854 ) ) ;
#2520 =( NAMED_UNIT ( * ) SI_UNIT ( $, .STERADIAN. ) SOLID_ANGLE_UNIT ( ) );
#2521 = LINE ( 'NONE', #2830, #2011 ) ;
#2522 = CARTESIAN_POINT ( 'NONE',  ( -8.500000000000001776, -9.407539813567788568E-16, 12.00000000000000000 ) ) ;
#2523 = AXIS2_PLACEMENT_3D ( 'NONE', #301, #1123, #1074 ) ;
#2524 = PLANE ( 'NONE',  #666 ) ;
#2525 = VERTEX_POINT ( 'NONE', #3867 ) ;
#2526 = LINE ( 'NONE', #2862, #4569 ) ;
#2527 = DIRECTION ( 'NONE',  ( -1.000000000000000000, 0.000000000000000000, 0.000000000000000000 ) ) ;
#2528 = DIRECTION ( 'NONE',  ( -0.000000000000000000, -0.000000000000000000, 1.000000000000000000 ) ) ;
#2529 = ORIENTED_EDGE ( 'NONE', *, *, #709, .T. ) ;
#2530 = EDGE_CURVE ( 'NONE', #2273, #121, #3543, .T. ) ;
#2531 = CARTESIAN_POINT ( 'NONE',  ( 2.000000000000000000, 0.8865213383406685965, -1.535500000000000753 ) ) ;
#2532 = LINE ( 'NONE', #2114, #2125 ) ;
#2533 = ADVANCED_FACE ( 'NONE', ( #3889 ), #3913, .T. ) ;
#2534 = EDGE_LOOP ( 'NONE', ( #3489, #434, #2007 ) ) ;
#2535 = CARTESIAN_POINT ( 'NONE',  ( 2.500000000000000000, -1.178949249685213863, 2.042000000000002924 ) ) ;
#2536 = DIRECTION ( 'NONE',  ( 0.000000000000000000, 0.000000000000000000, 1.000000000000000000 ) ) ;
#2537 = DIRECTION ( 'NONE',  ( -0.7071067811865306973, 0.000000000000000000, 0.7071067811865643371 ) ) ;
#2538 = ORIENTED_EDGE ( 'NONE', *, *, #1839, .T. ) ;
#2539 = ORIENTED_EDGE ( 'NONE', *, *, #541, .T. ) ;
#2540 = CARTESIAN_POINT ( 'NONE',  ( 0.000000000000000000, 0.000000000000000000, 0.000000000000000000 ) ) ;
#2541 = FACE_OUTER_BOUND ( 'NONE', #3135, .T. ) ;
#2542 = CARTESIAN_POINT ( 'NONE',  ( 22.30741055306794607, 11.28818263778244813, -19.99999999999996092 ) ) ;
#2543 = LINE ( 'NONE', #1409, #4586 ) ;
#2544 = ORIENTED_EDGE ( 'NONE', *, *, #4499, .T. ) ;
#2545 = CYLINDRICAL_SURFACE ( 'NONE', #1939, 3.500000000000000000 ) ;
#2546 = PLANE ( 'NONE',  #3360 ) ;
#2547 = CARTESIAN_POINT ( 'NONE',  ( 2.000000000000000000, 0.000000000000000000, 0.000000000000000000 ) ) ;
#2548 = ORIENTED_EDGE ( 'NONE', *, *, #709, .F. ) ;
#2549 = CARTESIAN_POINT ( 'NONE',  ( 19.30673457630776468, -12.50000000000007105, -12.00000000000000000 ) ) ;
#2550 = DIRECTION ( 'NONE',  ( 0.000000000000000000, -0.5000000000000011102, -0.8660254037844379305 ) ) ;
#2551 = PRODUCT_DEFINITION_FORMATION_WITH_SPECIFIED_SOURCE ( 'ANY', '', #1668, .NOT_KNOWN. ) ;
#2552 = DIRECTION ( 'NONE',  ( 1.000000000000000000, 0.000000000000000000, 0.000000000000000000 ) ) ;
#2553 = ORIENTED_EDGE ( 'NONE', *, *, #4499, .F. ) ;
#2554 = CIRCLE ( 'NONE', #1829, 6.999999999999999112 ) ;
#2555 = EDGE_CURVE ( 'NONE', #3396, #894, #2313, .T. ) ;
#2556 = EDGE_CURVE ( 'NONE', #107, #467, #4286, .T. ) ;
#2557 = FACE_OUTER_BOUND ( 'NONE', #1266, .T. ) ;
#2558 = FACE_OUTER_BOUND ( 'NONE', #2372, .T. ) ;
#2559 = AXIS2_PLACEMENT_3D ( 'NONE', #2503, #3554, #480 ) ;
#2560 = FACE_BOUND ( 'NONE', #1543, .T. ) ;
#2561 = ORIENTED_EDGE ( 'NONE', *, *, #2626, .F. ) ;
#2562 = EDGE_CURVE ( 'NONE', #1923, #1461, #1926, .T. ) ;
#2563 = AXIS2_PLACEMENT_3D ( 'NONE', #2203, #3030, #2646 ) ;
#2564 = CARTESIAN_POINT ( 'NONE',  ( 0.000000000000000000, 0.000000000000000000, 4.000000000000000000 ) ) ;
#2565 = DIRECTION ( 'NONE',  ( 0.000000000000000000, -0.4999999999999993894, 0.8660254037844389297 ) ) ;
#2566 = CARTESIAN_POINT ( 'NONE',  ( 0.000000000000000000, 0.000000000000000000, -32.00000000000000000 ) ) ;
#2567 = CARTESIAN_POINT ( 'NONE',  ( 12.50000000000000000, -1.383461737289380927E-15, 12.00000000000000000 ) ) ;
#2568 = CIRCLE ( 'NONE', #3678, 4.250000000000000000 ) ;
#2569 = VERTEX_POINT ( 'NONE', #4666 ) ;
#2570 = CARTESIAN_POINT ( 'NONE',  ( 15.00000000000000000, -16.00000000000000000, -26.00000000000000355 ) ) ;
#2571 = FACE_OUTER_BOUND ( 'NONE', #3553, .T. ) ;
#2572 = VECTOR ( 'NONE', #3148, 1000.000000000000114 ) ;
#2573 = CARTESIAN_POINT ( 'NONE',  ( 6.999999999999999112, 0.000000000000000000, -20.00000000000000000 ) ) ;
#2574 = AXIS2_PLACEMENT_3D ( 'NONE', #3023, #730, #1811 ) ;
#2575 = ORIENTED_EDGE ( 'NONE', *, *, #2760, .T. ) ;
#2576 = AXIS2_PLACEMENT_3D ( 'NONE', #1131, #677, #1450 ) ;
#2577 = AXIS2_PLACEMENT_3D ( 'NONE', #2868, #3170, #2038 ) ;
#2578 = CARTESIAN_POINT ( 'NONE',  ( 2.172477277502393807E-14, -16.00000000000000000, -23.90000000000000924 ) ) ;
#2579 = DIRECTION ( 'NONE',  ( 0.000000000000000000, 0.000000000000000000, -1.000000000000000000 ) ) ;
#2580 = AXIS2_PLACEMENT_3D ( 'NONE', #3050, #3791, #1892 ) ;
#2581 = AXIS2_PLACEMENT_3D ( 'NONE', #112, #2823, #2120 ) ;
#2582 = COLOUR_RGB ( '', 0.31764706, 0.68627451, 0.89019608) ;
#2583 = ORIENTED_EDGE ( 'NONE', *, *, #2305, .T. ) ;
#2584 = ADVANCED_FACE ( 'NONE', ( #471 ), #4688, .T. ) ;
#2585 = EDGE_CURVE ( 'NONE', #4766, #934, #4244, .T. ) ;
#2586 = AXIS2_PLACEMENT_3D ( 'NONE', #4358, #150, #1630 ) ;
#2587 = LINE ( 'NONE', #1100, #647 ) ;
#2588 = CARTESIAN_POINT ( 'NONE',  ( 25.00000000000000000, 0.000000000000000000, -20.00000000000000000 ) ) ;
#2589 = AXIS2_PLACEMENT_3D ( 'NONE', #197, #1692, #925 ) ;
#2590 = DIRECTION ( 'NONE',  ( -0.000000000000000000, -0.000000000000000000, -1.000000000000000000 ) ) ;
#2591 = ORIENTED_EDGE ( 'NONE', *, *, #1278, .F. ) ;
#2592 = ADVANCED_FACE ( 'NONE', ( #862 ), #4313, .T. ) ;
#2593 = AXIS2_PLACEMENT_3D ( 'NONE', #1909, #3047, #1562 ) ;
#2594 = FACE_OUTER_BOUND ( 'NONE', #3, .T. ) ;
#2595 = FACE_OUTER_BOUND ( 'NONE', #3374, .T. ) ;
#2596 = DIRECTION ( 'NONE',  ( -1.000000000000000000, 0.000000000000000000, 0.000000000000000000 ) ) ;
#2597 = VERTEX_POINT ( 'NONE', #2696 ) ;
#2598 = CARTESIAN_POINT ( 'NONE',  ( 2.000000000000000000, -1.329782007511006281, -0.7677499999999984892 ) ) ;
#2599 = EDGE_CURVE ( 'NONE', #153, #3209, #91, .T. ) ;
#2600 = ORIENTED_EDGE ( 'NONE', *, *, #869, .F. ) ;
#2601 = DIRECTION ( 'NONE',  ( -1.000000000000000000, -0.000000000000000000, -0.000000000000000000 ) ) ;
#2602 = CARTESIAN_POINT ( 'NONE',  ( 4.199999999999995737, 0.000000000000000000, 0.000000000000000000 ) ) ;
#2603 = AXIS2_PLACEMENT_3D ( 'NONE', #4880, #4195, #3819 ) ;
#2604 = CARTESIAN_POINT ( 'NONE',  ( 0.000000000000000000, 4.163799117101000559E-16, -3.299999999999999822 ) ) ;
#2605 = ORIENTED_EDGE ( 'NONE', *, *, #513, .F. ) ;
#2606 = DIRECTION ( 'NONE',  ( 0.000000000000000000, 0.000000000000000000, -1.000000000000000000 ) ) ;
#2607 = ITEM_DEFINED_TRANSFORMATION ( 'NONE', 'NONE', #3506,  #1918 ) ;
#2608 = CARTESIAN_POINT ( 'NONE',  ( 0.000000000000000000, -0.8865213383406690406, 1.535500000000000975 ) ) ;
#2609 = EDGE_LOOP ( 'NONE', ( #3090, #3803, #2605, #679, #1687 ) ) ;
#2610 = EDGE_CURVE ( 'NONE', #4618, #4395, #3492, .T. ) ;
#2611 = CARTESIAN_POINT ( 'NONE',  ( 2.500000000000000000, 2.357898499370433054, -1.951563910473907981E-15 ) ) ;
#2612 = CARTESIAN_POINT ( 'NONE',  ( 2.500000000000000000, 2.357898499370433054, -1.951563910473907981E-15 ) ) ;
#2613 = CARTESIAN_POINT ( 'NONE',  ( 2.000000000000000000, 1.773042676681340968, -2.276824562219559311E-15 ) ) ;
#2614 = CARTESIAN_POINT ( 'NONE',  ( -23.68543856465402797, 7.999999999999996447, 14.30577747056276472 ) ) ;
#2615 = VERTEX_POINT ( 'NONE', #521 ) ;
#2616 = DIRECTION ( 'NONE',  ( -0.000000000000000000, -0.000000000000000000, -1.000000000000000000 ) ) ;
#2617 = SURFACE_SIDE_STYLE ('',( #4133 ) ) ;
#2618 = CARTESIAN_POINT ( 'NONE',  ( 2.500000000000000000, 2.357898499370433054, -1.951563910473907981E-15 ) ) ;
#2619 = PLANE ( 'NONE',  #659 ) ;
#2620 = EDGE_CURVE ( 'NONE', #3659, #3812, #2045, .T. ) ;
#2621 = CARTESIAN_POINT ( 'NONE',  ( 8.500000000000003553, 21.37171027316251681, 4.000000000000000000 ) ) ;
#2622 = ORIENTED_EDGE ( 'NONE', *, *, #4228, .T. ) ;
#2623 = DIRECTION ( 'NONE',  ( 1.000000000000000000, 0.000000000000000000, -0.000000000000000000 ) ) ;
#2624 = EDGE_CURVE ( 'NONE', #1209, #4568, #970, .T. ) ;
#2625 = FACE_OUTER_BOUND ( 'NONE', #2609, .T. ) ;
#2626 = EDGE_CURVE ( 'NONE', #392, #4266, #2186, .T. ) ;
#2627 = EDGE_CURVE ( 'NONE', #987, #1875, #839, .T. ) ;
#2628 = ORIENTED_EDGE ( 'NONE', *, *, #3845, .F. ) ;
#2629 = CARTESIAN_POINT ( 'NONE',  ( 15.00000000000000000, -16.00000000000000000, -23.35000000000000853 ) ) ;
#2630 = ORIENTED_EDGE ( 'NONE', *, *, #646, .T. ) ;
#2631 = CYLINDRICAL_SURFACE ( 'NONE', #4817, 5.999999999999998224 ) ;
#2632 = CARTESIAN_POINT ( 'NONE',  ( -8.500000000000003553, 21.37171027316251681, 12.00000000000000000 ) ) ;
#2633 = CARTESIAN_POINT ( 'NONE',  ( 4.199999999999995737, 0.000000000000000000, 0.000000000000000000 ) ) ;
#2634 = DIRECTION ( 'NONE',  ( 1.000000000000000000, 1.106769389831504189E-16, -0.000000000000000000 ) ) ;
#2635 = ORIENTED_EDGE ( 'NONE', *, *, #2740, .T. ) ;
#2636 = CARTESIAN_POINT ( 'NONE',  ( -12.49999999999999822, -19.30673457630782863, 12.00000000000000000 ) ) ;
#2637 = AXIS2_PLACEMENT_3D ( 'NONE', #2226, #1769, #4834 ) ;
#2638 = CARTESIAN_POINT ( 'NONE',  ( -23.68543856465402797, 7.999999999999996447, -12.00000000000000000 ) ) ;
#2639 = LINE ( 'NONE', #2290, #1691 ) ;
#2640 = CARTESIAN_POINT ( 'NONE',  ( 22.21646894734066180, 11.46466559648295558, -31.93615172764430099 ) ) ;
#2641 = VERTEX_POINT ( 'NONE', #539 ) ;
#2642 = ORIENTED_EDGE ( 'NONE', *, *, #3742, .F. ) ;
#2643 = EDGE_CURVE ( 'NONE', #9, #4655, #3222, .T. ) ;
#2644 = ADVANCED_FACE ( 'NONE', ( #1748 ), #982, .F. ) ;
#2645 = DIRECTION ( 'NONE',  ( 0.000000000000000000, 0.000000000000000000, 1.000000000000000000 ) ) ;
#2646 = DIRECTION ( 'NONE',  ( 0.000000000000000000, 0.000000000000000000, 1.000000000000000000 ) ) ;
#2647 = PRODUCT_DEFINITION_SHAPE ( 'NONE', 'NONE',  #4970 ) ;
#2648 =( NAMED_UNIT ( * ) SI_UNIT ( $, .STERADIAN. ) SOLID_ANGLE_UNIT ( ) );
#2649 = VECTOR ( 'NONE', #1325, 1000.000000000000000 ) ;
#2650 = ORIENTED_EDGE ( 'NONE', *, *, #174, .T. ) ;
#2651 = EDGE_CURVE ( 'NONE', #537, #4618, #1368, .T. ) ;
#2652 = CONICAL_SURFACE ( 'NONE', #804, 2.041999999999999815, 1.047197551196591858 ) ;
#2653 = UNCERTAINTY_MEASURE_WITH_UNIT (LENGTH_MEASURE( 1.000000000000000082E-05 ), #1392, 'distance_accuracy_value', 'NONE');
#2654 = LINE ( 'NONE', #3060, #236 ) ;
#2655 = VECTOR ( 'NONE', #285, 1000.000000000000000 ) ;
#2656 = CIRCLE ( 'NONE', #3449, 2.649999999999985700 ) ;
#2657 = ORIENTED_EDGE ( 'NONE', *, *, #4083, .T. ) ;
#2658 = ADVANCED_FACE ( 'NONE', ( #230 ), #2090, .F. ) ;
#2659 = EDGE_CURVE ( 'NONE', #1875, #1889, #4088, .T. ) ;
#2660 = CIRCLE ( 'NONE', #4412, 5.999999999999998224 ) ;
#2661 = CIRCLE ( 'NONE', #2577, 23.00000000000000711 ) ;
#2662 = CARTESIAN_POINT ( 'NONE',  ( 22.47709430538512621, 10.94511065053865551, -29.23824484466006979 ) ) ;
#2663 = DIRECTION ( 'NONE',  ( 0.000000000000000000, 0.000000000000000000, -1.000000000000000000 ) ) ;
#2664 = DIRECTION ( 'NONE',  ( -0.000000000000000000, -0.000000000000000000, 1.000000000000000000 ) ) ;
#2665 = LINE ( 'NONE', #774, #183 ) ;
#2666 = VECTOR ( 'NONE', #799, 1000.000000000000000 ) ;
#2667 = APPLICATION_CONTEXT ( 'automotive_design' ) ;
#2668 = AXIS2_PLACEMENT_3D ( 'NONE', #2801, #4644, #3182 ) ;
#2669 = ORIENTED_EDGE ( 'NONE', *, *, #3042, .T. ) ;
#2670 = CARTESIAN_POINT ( 'NONE',  ( 0.000000000000000000, 0.000000000000000000, -12.00000000000000000 ) ) ;
#2671 = CARTESIAN_POINT ( 'NONE',  ( 0.000000000000000000, 0.000000000000000000, 0.000000000000000000 ) ) ;
#2672 = FACE_OUTER_BOUND ( 'NONE', #4327, .T. ) ;
#2673 = DIRECTION ( 'NONE',  ( 0.000000000000000000, 0.000000000000000000, -1.000000000000000000 ) ) ;
#2674 = CARTESIAN_POINT ( 'NONE',  ( -8.500000000000000000, -21.37171027316251681, 12.00000000000000000 ) ) ;
#2675 = ORIENTED_EDGE ( 'NONE', *, *, #2110, .F. ) ;
#2676 = VECTOR ( 'NONE', #3736, 1000.000000000000000 ) ;
#2677 = DIRECTION ( 'NONE',  ( 0.000000000000000000, 0.000000000000000000, -1.000000000000000000 ) ) ;
#2678 = DIRECTION ( 'NONE',  ( 1.000000000000000000, 0.000000000000000000, 0.000000000000000000 ) ) ;
#2679 = DIRECTION ( 'NONE',  ( 0.000000000000000000, 0.000000000000000000, 1.000000000000000000 ) ) ;
#2680 = ORIENTED_EDGE ( 'NONE', *, *, #3940, .F. ) ;
#2681 = AXIS2_PLACEMENT_3D ( 'NONE', #778, #2813, #408 ) ;
#2682 = CARTESIAN_POINT ( 'NONE',  ( -3.642919299551294898E-14, 16.00000000000000000, -23.35000000000000497 ) ) ;
#2683 = ORIENTED_EDGE ( 'NONE', *, *, #3297, .F. ) ;
#2684 = PRODUCT_DEFINITION ( 'UNKNOWN', '', #4463, #4938 ) ;
#2685 = ADVANCED_FACE ( 'NONE', ( #917 ), #4787, .T. ) ;
#2686 = ORIENTED_EDGE ( 'NONE', *, *, #3151, .F. ) ;
#2687 = CARTESIAN_POINT ( 'NONE',  ( 22.61871848390502393, 10.64917431867735154, -28.72182649103004692 ) ) ;
#2688 = CARTESIAN_POINT ( 'NONE',  ( 0.000000000000000000, 0.000000000000000000, 0.000000000000000000 ) ) ;
#2689 = ADVANCED_FACE ( 'NONE', ( #1350 ), #1710, .F. ) ;
#2690 = DIRECTION ( 'NONE',  ( 1.000000000000000000, -0.000000000000000000, -0.000000000000000000 ) ) ;
#2691 = CYLINDRICAL_SURFACE ( 'NONE', #2343, 2.099999999999997868 ) ;
#2692 = VERTEX_POINT ( 'NONE', #604 ) ;
#2693 = CARTESIAN_POINT ( 'NONE',  ( -3.666055405785289392E-14, -6.999999999999999112, -20.00000000000000000 ) ) ;
#2694 = DIRECTION ( 'NONE',  ( -1.000000000000000000, 0.000000000000000000, -6.982962677686266711E-15 ) ) ;
#2695 = LINE ( 'NONE', #4206, #3695 ) ;
#2696 = CARTESIAN_POINT ( 'NONE',  ( 22.03949535914419755, -11.80087472665740478, -30.28571428571428470 ) ) ;
#2697 = CARTESIAN_POINT ( 'NONE',  ( 21.96462198364264395, 11.94070939570634948, -30.42272372072263664 ) ) ;
#2698 = EDGE_LOOP ( 'NONE', ( #697, #1753, #246, #4017 ) ) ;
#2699 = ORIENTED_EDGE ( 'NONE', *, *, #655, .T. ) ;
#2700 = DIRECTION ( 'NONE',  ( 0.000000000000000000, 0.000000000000000000, 1.000000000000000000 ) ) ;
#2701 = DIRECTION ( 'NONE',  ( 1.000000000000000000, -0.000000000000000000, -0.000000000000000000 ) ) ;
#2702 = FACE_OUTER_BOUND ( 'NONE', #37, .T. ) ;
#2703 = DIRECTION ( 'NONE',  ( 0.000000000000000000, 1.000000000000000000, -1.467581828789149532E-15 ) ) ;
#2704 = ORIENTED_EDGE ( 'NONE', *, *, #1154, .F. ) ;
#2705 = UNCERTAINTY_MEASURE_WITH_UNIT (LENGTH_MEASURE( 1.000000000000000082E-05 ), #2021, 'distance_accuracy_value', 'NONE');
#2706 = DIRECTION ( 'NONE',  ( 1.000000000000000000, 0.000000000000000000, 0.000000000000000000 ) ) ;
#2707 = CARTESIAN_POINT ( 'NONE',  ( -6.708203932499367639, 2.000000000000001332, -32.00000000000000000 ) ) ;
#2708 = VERTEX_POINT ( 'NONE', #209 ) ;
#2709 = VERTEX_POINT ( 'NONE', #2516 ) ;
#2710 = FACE_OUTER_BOUND ( 'NONE', #3156, .T. ) ;
#2711 = PLANE ( 'NONE',  #895 ) ;
#2712 = FACE_OUTER_BOUND ( 'NONE', #48, .T. ) ;
#2713 = EDGE_LOOP ( 'NONE', ( #360, #2087, #1277, #3673 ) ) ;
#2714 = ADVANCED_FACE ( 'NONE', ( #3248 ), #582, .T. ) ;
#2715 = DIRECTION ( 'NONE',  ( 6.982962677686266711E-15, 0.000000000000000000, -1.000000000000000000 ) ) ;
#2716 = CARTESIAN_POINT ( 'NONE',  ( 0.000000000000000000, 0.000000000000000000, -32.00000000000000000 ) ) ;
#2717 = CARTESIAN_POINT ( 'NONE',  ( 2.000000000000000000, 0.000000000000000000, 0.000000000000000000 ) ) ;
#2718 = DIRECTION ( 'NONE',  ( 1.357798298438996130E-15, -1.000000000000000000, 0.000000000000000000 ) ) ;
#2719 = EDGE_LOOP ( 'NONE', ( #4535, #160, #1611, #3257 ) ) ;
#2720 = CIRCLE ( 'NONE', #2405, 6.999999999999999112 ) ;
#2721 = EDGE_LOOP ( 'NONE', ( #4798, #3582 ) ) ;
#2722 = SHAPE_REPRESENTATION_RELATIONSHIP ( 'NONE' , 'NONE' ,  #1644, #38 ) ;
#2723 = CARTESIAN_POINT ( 'NONE',  ( 0.2500000000000002220, 0.000000000000000000, 0.000000000000000000 ) ) ;
#2724 = PLANE ( 'NONE',  #2432 ) ;
#2725 = CARTESIAN_POINT ( 'NONE',  ( 2.500000000000000000, -1.178949249685213863, 2.042000000000002924 ) ) ;
#2726 = CIRCLE ( 'NONE', #1205, 22.99999999999998934 ) ;
#2727 = VERTEX_POINT ( 'NONE', #4743 ) ;
#2728 = CARTESIAN_POINT ( 'NONE',  ( 2.500000000000000000, -2.357898499370432610, 3.252606517456513302E-15 ) ) ;
#2729 = LINE ( 'NONE', #4247, #4803 ) ;
#2730 = VECTOR ( 'NONE', #2864, 1000.000000000000227 ) ;
#2731 = ORIENTED_EDGE ( 'NONE', *, *, #628, .T. ) ;
#2732 = ORIENTED_EDGE ( 'NONE', *, *, #986, .F. ) ;
#2733 = VECTOR ( 'NONE', #762, 1000.000000000000000 ) ;
#2734 = PRODUCT_DEFINITION_CONTEXT ( 'detailed design', #1723, 'design' ) ;
#2735 = VECTOR ( 'NONE', #3463, 1000.000000000000000 ) ;
#2736 = CARTESIAN_POINT ( 'NONE',  ( 22.90825000241674303, -10.01062433489519954, -26.41097745015308718 ) ) ;
#2737 = CONICAL_SURFACE ( 'NONE', #4811, 1.610000000000000098, 0.7853981633974647103 ) ;
#2738 = DIRECTION ( 'NONE',  ( -1.000000000000000000, -0.000000000000000000, -0.000000000000000000 ) ) ;
#2739 = DIRECTION ( 'NONE',  ( -0.000000000000000000, -0.000000000000000000, -1.000000000000000000 ) ) ;
#2740 = EDGE_CURVE ( 'NONE', #1594, #3321, #3585, .T. ) ;
#2741 = ORIENTED_EDGE ( 'NONE', *, *, #228, .T. ) ;
#2742 = EDGE_LOOP ( 'NONE', ( #769, #1367, #98, #4777, #16 ) ) ;
#2743 = VECTOR ( 'NONE', #2067, 1000.000000000000000 ) ;
#2744 = AXIS2_PLACEMENT_3D ( 'NONE', #3706, #2230, #1778 ) ;
#2745 = CARTESIAN_POINT ( 'NONE',  ( 0.000000000000000000, 0.000000000000000000, -4.000000000000000000 ) ) ;
#2746 = DIRECTION ( 'NONE',  ( 0.000000000000000000, 0.000000000000000000, -1.000000000000000000 ) ) ;
#2747 = AXIS2_PLACEMENT_3D ( 'NONE', #3345, #2677, #4872 ) ;
#2748 = AXIS2_PLACEMENT_3D ( 'NONE', #4689, #3586, #886 ) ;
#2749 = CARTESIAN_POINT ( 'NONE',  ( 21.87533763385574659, 12.10248395817102107, -30.91117611071771165 ) ) ;
#2750 = ADVANCED_FACE ( 'NONE', ( #4713 ), #4033, .F. ) ;
#2751 = EDGE_CURVE ( 'NONE', #865, #536, #815, .T. ) ;
#2752 = ORIENTED_EDGE ( 'NONE', *, *, #1510, .T. ) ;
#2753 = AXIS2_PLACEMENT_3D ( 'NONE', #4272, #1076, #4521 ) ;
#2754 = ORIENTED_EDGE ( 'NONE', *, *, #2898, .F. ) ;
#2755 = B_SPLINE_CURVE_WITH_KNOTS ( 'NONE', 3,
 ( #4449, #4150, #1878, #4839, #1026, #4076, #2187, #284, #1805, #797, #464, #3823, #831, #3456, #25, #3858, #2281, #3485, #437, #2687, #3904, #2662, #1979, #1959, #3036 ),
 .UNSPECIFIED., .F., .F.,
 ( 4, 2, 2, 2, 2, 2, 1, 2, 2, 2, 2, 2, 4 ),
 ( 0.005424949174462414224, 0.006631086198200492922, 0.007234154710069537475, 0.007837223221938582896, 0.009043360245676663328, 0.009646428757545708749, 0.01024949726941475417, 0.01085256578128379785, 0.01145563429315284328, 0.01266177131689092197, 0.01326483982875995699, 0.01386790834062899200, 0.01507404536436706549 ),
 .UNSPECIFIED. ) ;
#2756 =( NAMED_UNIT ( * ) PLANE_ANGLE_UNIT ( ) SI_UNIT ( $, .RADIAN. ) );
#2757 = CARTESIAN_POINT ( 'NONE',  ( 23.00000000000000711, 2.816687638038913141E-15, 4.000000000000000000 ) ) ;
#2758 = LINE ( 'NONE', #527, #2831 ) ;
#2759 = CARTESIAN_POINT ( 'NONE',  ( -31.74999999999995737, 0.000000000000000000, 0.000000000000000000 ) ) ;
#2760 = EDGE_CURVE ( 'NONE', #3989, #3847, #176, .T. ) ;
#2761 = AXIS2_PLACEMENT_3D ( 'NONE', #4040, #3394, #611 ) ;
#2762 = VERTEX_POINT ( 'NONE', #4056 ) ;
#2763 = DIRECTION ( 'NONE',  ( -1.000000000000000000, 3.357200482488896896E-15, 0.000000000000000000 ) ) ;
#2764 = CARTESIAN_POINT ( 'NONE',  ( 0.000000000000000000, 0.000000000000000000, 4.000000000000000000 ) ) ;
#2765 = VERTEX_POINT ( 'NONE', #2872 ) ;
#2766 = ORIENTED_EDGE ( 'NONE', *, *, #487, .F. ) ;
#2767 = CARTESIAN_POINT ( 'NONE',  ( 22.47709430538511910, -10.94511065053865373, -22.76175515533994087 ) ) ;
#2768 = SURFACE_STYLE_FILL_AREA ( #1235 ) ;
#2769 = DIRECTION ( 'NONE',  ( -1.000000000000000000, -0.000000000000000000, -0.000000000000000000 ) ) ;
#2770 = ORIENTED_EDGE ( 'NONE', *, *, #4437, .T. ) ;
#2771 = ORIENTED_EDGE ( 'NONE', *, *, #1279, .F. ) ;
#2772 = APPLICATION_PROTOCOL_DEFINITION ( 'draft international standard', 'automotive_design', 1998, #3945 ) ;
#2773 = DIRECTION ( 'NONE',  ( -1.000000000000000000, 0.000000000000000000, 0.000000000000000000 ) ) ;
#2774 = DIRECTION ( 'NONE',  ( 0.000000000000000000, 0.000000000000000000, -1.000000000000000000 ) ) ;
#2775 = CARTESIAN_POINT ( 'NONE',  ( 15.00000000000000000, -20.00000000000000355, -32.00000000000000000 ) ) ;
#2776 = EDGE_LOOP ( 'NONE', ( #1894, #2048, #2173, #3511, #4833 ) ) ;
#2777 = ADVANCED_FACE ( 'NONE', ( #625, #1288 ), #4384, .F. ) ;
#2778 = DIRECTION ( 'NONE',  ( -0.000000000000000000, -0.000000000000000000, -1.000000000000000000 ) ) ;
#2779 = PRODUCT_DEFINITION_SHAPE ( 'NONE', 'NONE',  #4965 ) ;
#2780 = CARTESIAN_POINT ( 'NONE',  ( 0.000000000000000000, 0.000000000000000000, 12.00000000000000000 ) ) ;
#2781 = CARTESIAN_POINT ( 'NONE',  ( -25.00000000000000000, 3.061616997868383043E-15, -20.00000000000000000 ) ) ;
#2782 = VERTEX_POINT ( 'NONE', #3679 ) ;
#2783 = ADVANCED_FACE ( 'NONE', ( #560, #956 ), #358, .T. ) ;
#2784 = CARTESIAN_POINT ( 'NONE',  ( 4.199999999999995737, 0.000000000000000000, 0.000000000000000000 ) ) ;
#2785 = DIRECTION ( 'NONE',  ( -0.000000000000000000, -0.000000000000000000, 1.000000000000000000 ) ) ;
#2786 = ORIENTED_EDGE ( 'NONE', *, *, #4081, .T. ) ;
#2787 = ORIENTED_EDGE ( 'NONE', *, *, #1787, .T. ) ;
#2788 = ADVANCED_FACE ( 'NONE', ( #4078 ), #3731, .T. ) ;
#2789 = DIRECTION ( 'NONE',  ( 0.000000000000000000, 0.000000000000000000, -1.000000000000000000 ) ) ;
#2790 = SURFACE_STYLE_FILL_AREA ( #2116 ) ;
#2791 = DIRECTION ( 'NONE',  ( -0.000000000000000000, -0.000000000000000000, 1.000000000000000000 ) ) ;
#2792 = DIRECTION ( 'NONE',  ( -1.000000000000000000, -0.000000000000000000, -0.000000000000000000 ) ) ;
#2793 = EDGE_LOOP ( 'NONE', ( #1956, #1348, #3817, #859 ) ) ;
#2794 = EDGE_LOOP ( 'NONE', ( #2355, #2926, #702, #4624, #3618 ) ) ;
#2795 = FACE_OUTER_BOUND ( 'NONE', #2698, .T. ) ;
#2796 = CARTESIAN_POINT ( 'NONE',  ( 0.1999999999999987899, 4.041334437186265510E-16, -3.299999999999999822 ) ) ;
#2797 = DIRECTION ( 'NONE',  ( -1.000000000000000000, -0.000000000000000000, -0.000000000000000000 ) ) ;
#2798 = ORIENTED_EDGE ( 'NONE', *, *, #1643, .F. ) ;
#2799 = ORIENTED_EDGE ( 'NONE', *, *, #4367, .T. ) ;
#2800 = DIRECTION ( 'NONE',  ( 1.000000000000000000, 0.000000000000000000, 0.000000000000000000 ) ) ;
#2801 = CARTESIAN_POINT ( 'NONE',  ( -7.332110811570578784E-14, -6.999999999999999112, -32.00000000000000000 ) ) ;
#2802 = DIRECTION ( 'NONE',  ( 1.000000000000000000, 0.000000000000000000, 0.000000000000000000 ) ) ;
#2803 = EDGE_CURVE ( 'NONE', #3027, #3976, #1806, .T. ) ;
#2804 = ORIENTED_EDGE ( 'NONE', *, *, #3153, .F. ) ;
#2805 = VECTOR ( 'NONE', #2838, 1000.000000000000000 ) ;
#2806 = CARTESIAN_POINT ( 'NONE',  ( -9.000000000000001776, 2.000000000000000000, -12.00000000000000000 ) ) ;
#2807 = CARTESIAN_POINT ( 'NONE',  ( 2.000000000000000000, -0.8865213383406690406, 1.535500000000000975 ) ) ;
#2808 = AXIS2_PLACEMENT_3D ( 'NONE', #2602, #2904, #4420 ) ;
#2809 = ORIENTED_EDGE ( 'NONE', *, *, #3468, .T. ) ;
#2810 = EDGE_CURVE ( 'NONE', #45, #4182, #329, .T. ) ;
#2811 = VERTEX_POINT ( 'NONE', #1081 ) ;
#2812 = CIRCLE ( 'NONE', #1922, 23.00000000000000711 ) ;
#2813 = DIRECTION ( 'NONE',  ( 0.000000000000000000, 0.8660254037844380415, -0.5000000000000011102 ) ) ;
#2814 = LINE ( 'NONE', #4658, #1307 ) ;
#2815 = DIRECTION ( 'NONE',  ( 1.000000000000000000, 0.000000000000000000, 0.000000000000000000 ) ) ;
#2816 = EDGE_CURVE ( 'NONE', #1313, #4859, #1827, .T. ) ;
#2817 = AXIS2_PLACEMENT_3D ( 'NONE', #2451, #988, #3615 ) ;
#2818 = ORIENTED_EDGE ( 'NONE', *, *, #4660, .F. ) ;
#2819 = ORIENTED_EDGE ( 'NONE', *, *, #2472, .T. ) ;
#2820 = VECTOR ( 'NONE', #4894, 1000.000000000000000 ) ;
#2821 = CARTESIAN_POINT ( 'NONE',  ( 2.000000000000000000, -1.773042676681340968, 2.059984127722458425E-15 ) ) ;
#2822 = DIRECTION ( 'NONE',  ( -0.000000000000000000, -0.000000000000000000, 1.000000000000000000 ) ) ;
#2823 = DIRECTION ( 'NONE',  ( -0.000000000000000000, -0.000000000000000000, 1.000000000000000000 ) ) ;
#2824 = AXIS2_PLACEMENT_3D ( 'NONE', #2163, #2822, #4814 ) ;
#2825 = AXIS2_PLACEMENT_3D ( 'NONE', #1079, #3780, #2162 ) ;
#2826 = ORIENTED_EDGE ( 'NONE', *, *, #2740, .F. ) ;
#2827 = VERTEX_POINT ( 'NONE', #4152 ) ;
#2828 = AXIS2_PLACEMENT_3D ( 'NONE', #3301, #4829, #4439 ) ;
#2829 = VECTOR ( 'NONE', #3337, 1000.000000000000000 ) ;
#2830 = CARTESIAN_POINT ( 'NONE',  ( -23.68543856465402797, 7.999999999999996447, 14.30577747056276472 ) ) ;
#2831 = VECTOR ( 'NONE', #63, 1000.000000000000000 ) ;
#2832 = CARTESIAN_POINT ( 'NONE',  ( 6.999999999999999112, 0.000000000000000000, -12.00000000000000000 ) ) ;
#2833 = DIRECTION ( 'NONE',  ( -0.000000000000000000, -0.000000000000000000, 1.000000000000000000 ) ) ;
#2834 = VERTEX_POINT ( 'NONE', #724 ) ;
#2835 = AXIS2_PLACEMENT_3D ( 'NONE', #2441, #128, #3189 ) ;
#2836 =( REPRESENTATION_RELATIONSHIP ('NONE','NONE', #137, #4748 ) REPRESENTATION_RELATIONSHIP_WITH_TRANSFORMATION ( #2933 )SHAPE_REPRESENTATION_RELATIONSHIP( ) );
#2837 = AXIS2_PLACEMENT_3D ( 'NONE', #2717, #4232, #4264 ) ;
#2838 = DIRECTION ( 'NONE',  ( -1.000000000000000000, 0.000000000000000000, 0.000000000000000000 ) ) ;
#2839 = EDGE_CURVE ( 'NONE', #645, #1395, #3408, .T. ) ;
#2840 = DIRECTION ( 'NONE',  ( 0.000000000000000000, 0.000000000000000000, 1.000000000000000000 ) ) ;
#2841 = CIRCLE ( 'NONE', #1865, 2.500000000000000888 ) ;
#2842 = ORIENTED_EDGE ( 'NONE', *, *, #2276, .F. ) ;
#2843 = CONICAL_SURFACE ( 'NONE', #2192, 25.00000000000000000, 0.7853981633974500554 ) ;
#2844 = DIRECTION ( 'NONE',  ( -1.000000000000000000, 0.000000000000000000, 0.000000000000000000 ) ) ;
#2845 = EDGE_CURVE ( 'NONE', #3988, #3154, #4451, .T. ) ;
#2846 = DIRECTION ( 'NONE',  ( -0.000000000000000000, -0.000000000000000000, 1.000000000000000000 ) ) ;
#2847 = DIRECTION ( 'NONE',  ( 0.000000000000000000, 0.000000000000000000, -1.000000000000000000 ) ) ;
#2848 = ORIENTED_EDGE ( 'NONE', *, *, #4669, .F. ) ;
#2849 = ORIENTED_EDGE ( 'NONE', *, *, #3475, .F. ) ;
#2850 = AXIS2_PLACEMENT_3D ( 'NONE', #1022, #949, #2183 ) ;
#2851 = ADVANCED_FACE ( 'NONE', ( #1855 ), #3293, .F. ) ;
#2852 = EDGE_CURVE ( 'NONE', #4670, #586, #1424, .T. ) ;
#2853 = CARTESIAN_POINT ( 'NONE',  ( 0.000000000000000000, -2.357898499370432610, 3.252606517456513302E-15 ) ) ;
#2854 = DIRECTION ( 'NONE',  ( -1.000000000000000000, 4.336808689942018722E-16, 0.000000000000000000 ) ) ;
#2855 = DIRECTION ( 'NONE',  ( 0.000000000000000000, -0.4999999999999993339, 0.8660254037844389297 ) ) ;
#2856 = VERTEX_POINT ( 'NONE', #1497 ) ;
#2857 = ORIENTED_EDGE ( 'NONE', *, *, #3897, .T. ) ;
#2858 =( NAMED_UNIT ( * ) SI_UNIT ( $, .STERADIAN. ) SOLID_ANGLE_UNIT ( ) );
#2859 = FACE_OUTER_BOUND ( 'NONE', #3243, .T. ) ;
#2860 = LINE ( 'NONE', #565, #2176 ) ;
#2861 = ORIENTED_EDGE ( 'NONE', *, *, #1577, .F. ) ;
#2862 = CARTESIAN_POINT ( 'NONE',  ( 2.000000000000000000, -0.8865213383406721492, -1.535499999999999199 ) ) ;
#2863 = DIRECTION ( 'NONE',  ( -1.000000000000000000, -0.000000000000000000, -0.000000000000000000 ) ) ;
#2864 = DIRECTION ( 'NONE',  ( 0.000000000000000000, -0.5000000000000008882, -0.8660254037844380415 ) ) ;
#2865 = EDGE_LOOP ( 'NONE', ( #2787, #2373, #864, #821 ) ) ;
#2866 = DIRECTION ( 'NONE',  ( -0.000000000000000000, -0.000000000000000000, -1.000000000000000000 ) ) ;
#2867 = SHAPE_DEFINITION_REPRESENTATION ( #812, #137 ) ;
#2868 = CARTESIAN_POINT ( 'NONE',  ( 0.000000000000000000, 0.000000000000000000, 4.000000000000000000 ) ) ;
#2869 = ORIENTED_EDGE ( 'NONE', *, *, #800, .T. ) ;
#2870 = EDGE_CURVE ( 'NONE', #1919, #881, #1933, .T. ) ;
#2871 = CARTESIAN_POINT ( 'NONE',  ( 0.1999999999999987899, 0.000000000000000000, 0.000000000000000000 ) ) ;
#2872 = CARTESIAN_POINT ( 'NONE',  ( -21.37171027316247063, 8.500000000000072831, -12.00000000000000000 ) ) ;
#2873 = CARTESIAN_POINT ( 'NONE',  ( 0.000000000000000000, 0.8865213383406717051, 1.535499999999998533 ) ) ;
#2874 = ORIENTED_EDGE ( 'NONE', *, *, #1745, .F. ) ;
#2875 =( GEOMETRIC_REPRESENTATION_CONTEXT ( 3 ) GLOBAL_UNCERTAINTY_ASSIGNED_CONTEXT ( ( #2705 ) ) GLOBAL_UNIT_ASSIGNED_CONTEXT ( ( #2021, #2756, #1219 ) ) REPRESENTATION_CONTEXT ( 'NONE', 'WORKASPACE' ) );
#2876 = ORIENTED_EDGE ( 'NONE', *, *, #907, .F. ) ;
#2877 = DIRECTION ( 'NONE',  ( 1.000000000000000000, 0.000000000000000000, 0.000000000000000000 ) ) ;
#2878 = LINE ( 'NONE', #3252, #4742 ) ;
#2879 = FACE_OUTER_BOUND ( 'NONE', #3495, .T. ) ;
#2880 = EDGE_LOOP ( 'NONE', ( #4392, #1513, #3048 ) ) ;
#2881 = DIRECTION ( 'NONE',  ( 1.000000000000000000, 0.000000000000000000, 0.000000000000000000 ) ) ;
#2882 = CARTESIAN_POINT ( 'NONE',  ( 15.00000000000000000, 16.00000000000000000, -28.64999999999999503 ) ) ;
#2883 = ORIENTED_EDGE ( 'NONE', *, *, #2905, .T. ) ;
#2884 = VECTOR ( 'NONE', #4194, 1000.000000000000000 ) ;
#2885 = FACE_OUTER_BOUND ( 'NONE', #4922, .T. ) ;
#2886 = DIRECTION ( 'NONE',  ( -0.000000000000000000, -0.000000000000000000, -1.000000000000000000 ) ) ;
#2887 = ORIENTED_EDGE ( 'NONE', *, *, #4724, .F. ) ;
#2888 = CARTESIAN_POINT ( 'NONE',  ( -3.041771206386918902E-14, -8.500000000000001776, -12.00000000000000000 ) ) ;
#2889 = CONICAL_SURFACE ( 'NONE', #4640, 1.535500000000000087, 1.047197551196590748 ) ;
#2890 = CARTESIAN_POINT ( 'NONE',  ( 0.000000000000000000, 0.000000000000000000, -20.00000000000000000 ) ) ;
#2891 = LINE ( 'NONE', #3286, #652 ) ;
#2892 = ORIENTED_EDGE ( 'NONE', *, *, #4604, .T. ) ;
#2893 = CIRCLE ( 'NONE', #3601, 0.2000000000000000944 ) ;
#2894 = ORIENTED_EDGE ( 'NONE', *, *, #2620, .F. ) ;
#2895 = DIRECTION ( 'NONE',  ( 0.000000000000000000, -0.4999999999999993894, 0.8660254037844389297 ) ) ;
#2896 = PRODUCT_DEFINITION ( 'UNKNOWN', '', #4064, #3238 ) ;
#2897 = CARTESIAN_POINT ( 'NONE',  ( -15.26180729995780716, -16.00000000000000355, -26.00000000000000355 ) ) ;
#2898 = EDGE_CURVE ( 'NONE', #4346, #3611, #1134, .T. ) ;
#2899 = CIRCLE ( 'NONE', #1220, 2.500000000000000888 ) ;
#2900 = DIRECTION ( 'NONE',  ( -1.000000000000000000, 4.336808689942018722E-16, 0.000000000000000000 ) ) ;
#2901 = AXIS2_PLACEMENT_3D ( 'NONE', #2071, #2097, #161 ) ;
#2902 = ORIENTED_EDGE ( 'NONE', *, *, #4579, .F. ) ;
#2903 = VECTOR ( 'NONE', #2334, 1000.000000000000000 ) ;
#2904 = DIRECTION ( 'NONE',  ( 1.000000000000000000, 0.000000000000000000, 0.000000000000000000 ) ) ;
#2905 = EDGE_CURVE ( 'NONE', #4296, #645, #1767, .T. ) ;
#2906 = LINE ( 'NONE', #4421, #2730 ) ;
#2907 = ADVANCED_FACE ( 'NONE', ( #1475 ), #649, .F. ) ;
#2908 = AXIS2_PLACEMENT_3D ( 'NONE', #4178, #1960, #1879 ) ;
#2909 = AXIS2_PLACEMENT_3D ( 'NONE', #1403, #2938, #4503 ) ;
#2910 = ORIENTED_EDGE ( 'NONE', *, *, #2205, .F. ) ;
#2911 = CARTESIAN_POINT ( 'NONE',  ( -23.68543856465402442, -8.000000000000003553, 14.30577747056276472 ) ) ;
#2912 = CIRCLE ( 'NONE', #3309, 25.00000000000000000 ) ;
#2913 = CARTESIAN_POINT ( 'NONE',  ( -11.26180729995789775, 15.99999999999999645, -26.00000000000000355 ) ) ;
#2914 = EDGE_LOOP ( 'NONE', ( #2308, #138, #1065, #397 ) ) ;
#2915 = CLOSED_SHELL ( 'NONE', ( #2112, #4054, #1571, #421, #4696, #4380, #18, #1019, #914, #1596, #3329, #954, #4447, #1338, #4145, #4756, #2685, #2991, #2644, #3026, #4697, #2197, #3781, #1871, #3444, #1726, #2584, #2111, #2750, #3142, #352, #4875 ) ) ;
#2916 = CIRCLE ( 'NONE', #745, 23.00000000000000711 ) ;
#2917 = FACE_OUTER_BOUND ( 'NONE', #4628, .T. ) ;
#2918 = DIRECTION ( 'NONE',  ( -3.357200482488897685E-15, -1.000000000000000000, 0.000000000000000000 ) ) ;
#2919 = VERTEX_POINT ( 'NONE', #2188 ) ;
#2920 = DIRECTION ( 'NONE',  ( 0.000000000000000000, 0.000000000000000000, -1.000000000000000000 ) ) ;
#2921 = DIRECTION ( 'NONE',  ( -1.000000000000000000, 0.000000000000000000, 0.000000000000000000 ) ) ;
#2922 =( REPRESENTATION_RELATIONSHIP ('NONE','NONE', #137, #1326 ) REPRESENTATION_RELATIONSHIP_WITH_TRANSFORMATION ( #250 )SHAPE_REPRESENTATION_RELATIONSHIP( ) );
#2923 = LINE ( 'NONE', #3971, #4328 ) ;
#2924 = DIRECTION ( 'NONE',  ( -0.000000000000000000, -0.000000000000000000, 1.000000000000000000 ) ) ;
#2925 = ORIENTED_EDGE ( 'NONE', *, *, #288, .F. ) ;
#2926 = ORIENTED_EDGE ( 'NONE', *, *, #3052, .F. ) ;
#2927 = CARTESIAN_POINT ( 'NONE',  ( 21.37171027316246708, -8.500000000000078160, -12.00000000000000000 ) ) ;
#2928 = CARTESIAN_POINT ( 'NONE',  ( 22.03949535914419755, -11.80087472665740478, -30.28571428571428470 ) ) ;
#2929 = VERTEX_POINT ( 'NONE', #4179 ) ;
#2930 = EDGE_CURVE ( 'NONE', #3315, #1209, #2899, .T. ) ;
#2931 = LINE ( 'NONE', #1000, #4226 ) ;
#2932 = DIRECTION ( 'NONE',  ( -1.000000000000000000, 3.357200482488897290E-15, 0.000000000000000000 ) ) ;
#2933 = ITEM_DEFINED_TRANSFORMATION ( 'NONE', 'NONE', #4703,  #1918 ) ;
#2934 = ORIENTED_EDGE ( 'NONE', *, *, #2253, .F. ) ;
#2935 = ADVANCED_FACE ( 'NONE', ( #2558 ), #3017, .F. ) ;
#2936 = DIRECTION ( 'NONE',  ( 0.000000000000000000, 0.000000000000000000, -1.000000000000000000 ) ) ;
#2937 = DIRECTION ( 'NONE',  ( -1.000000000000000000, -0.000000000000000000, -0.000000000000000000 ) ) ;
#2938 = DIRECTION ( 'NONE',  ( 0.000000000000000000, 0.000000000000000000, 1.000000000000000000 ) ) ;
#2939 = ORIENTED_EDGE ( 'NONE', *, *, #849, .T. ) ;
#2940 = ORIENTED_EDGE ( 'NONE', *, *, #1703, .F. ) ;
#2941 = LINE ( 'NONE', #2618, #1049 ) ;
#2942 = CARTESIAN_POINT ( 'NONE',  ( 15.00000000000000000, -16.00000000000000000, -26.00000000000000355 ) ) ;
#2943 = ORIENTED_EDGE ( 'NONE', *, *, #749, .T. ) ;
#2944 = LINE ( 'NONE', #705, #191 ) ;
#2945 = VERTEX_POINT ( 'NONE', #2283 ) ;
#2946 = PRESENTATION_LAYER_ASSIGNMENT (  '', '', ( #4945 ) ) ;
#2947 = ORIENTED_EDGE ( 'NONE', *, *, #2167, .F. ) ;
#2948 = CARTESIAN_POINT ( 'NONE',  ( 2.000000000000000000, 1.773042676681340968, -2.276824562219559311E-15 ) ) ;
#2949 = DIRECTION ( 'NONE',  ( 0.000000000000000000, 0.000000000000000000, -1.000000000000000000 ) ) ;
#2950 = DIRECTION ( 'NONE',  ( 1.000000000000000000, -0.000000000000000000, -0.000000000000000000 ) ) ;
#2951 = AXIS2_PLACEMENT_3D ( 'NONE', #1754, #3290, #1010 ) ;
#2952 = EDGE_CURVE ( 'NONE', #4685, #675, #4565, .T. ) ;
#2953 = VERTEX_POINT ( 'NONE', #2588 ) ;
#2954 = DIRECTION ( 'NONE',  ( 1.000000000000000000, -0.000000000000000000, -0.000000000000000000 ) ) ;
#2955 = LINE ( 'NONE', #573, #4274 ) ;
#2956 = PRESENTATION_STYLE_ASSIGNMENT (( #4398 ) ) ;
#2957 = ADVANCED_FACE ( 'NONE', ( #4585 ), #3086, .F. ) ;
#2958 = ORIENTED_EDGE ( 'NONE', *, *, #1254, .F. ) ;
#2959 = VECTOR ( 'NONE', #1623, 1000.000000000000000 ) ;
#2960 = DIRECTION ( 'NONE',  ( 3.578554360455198522E-15, 1.000000000000000000, 0.000000000000000000 ) ) ;
#2961 = EDGE_CURVE ( 'Edge1', #2762, #4063, #2499, .T. ) ;
#2962 = ADVANCED_FACE ( 'NONE', ( #1901 ), #2711, .F. ) ;
#2963 = DIRECTION ( 'NONE',  ( 0.000000000000000000, 0.000000000000000000, 1.000000000000000000 ) ) ;
#2964 = AXIS2_PLACEMENT_3D ( 'NONE', #3255, #1670, #965 ) ;
#2965 = LINE ( 'NONE', #3680, #4094 ) ;
#2966 = ORIENTED_EDGE ( 'NONE', *, *, #880, .T. ) ;
#2967 = VECTOR ( 'NONE', #481, 999.9999999999998863 ) ;
#2968 = DIRECTION ( 'NONE',  ( 0.000000000000000000, 0.000000000000000000, -1.000000000000000000 ) ) ;
#2969 = FILL_AREA_STYLE ('',( #4456 ) ) ;
#2970 = FACE_OUTER_BOUND ( 'NONE', #482, .T. ) ;
#2971 = CARTESIAN_POINT ( 'NONE',  ( 2.500000000000000000, 1.768423874527822681, -1.021000000000002794 ) ) ;
#2972 = CARTESIAN_POINT ( 'NONE',  ( 4.196500603111122875E-14, 12.50000000000000178, -4.000000000000000000 ) ) ;
#2973 = CIRCLE ( 'NONE', #4476, 22.99999999999998934 ) ;
#2974 = VERTEX_POINT ( 'NONE', #773 ) ;
#2975 = LINE ( 'NONE', #4501, #578 ) ;
#2976 = CARTESIAN_POINT ( 'NONE',  ( 0.000000000000000000, 0.000000000000000000, -12.00000000000000000 ) ) ;
#2977 = VECTOR ( 'NONE', #1264, 1000.000000000000000 ) ;
#2978 = DIRECTION ( 'NONE',  ( 0.000000000000000000, 0.000000000000000000, -1.000000000000000000 ) ) ;
#2979 = VECTOR ( 'NONE', #2265, 1000.000000000000000 ) ;
#2980 = EDGE_LOOP ( 'NONE', ( #211, #4486, #706, #789 ) ) ;
#2981 = VECTOR ( 'NONE', #3801, 1000.000000000000000 ) ;
#2982 = TOROIDAL_SURFACE ( 'NONE', #3610, 2.700000000000001066, 0.2000000000000000111 ) ;
#2983 = EDGE_CURVE ( 'NONE', #1202, #754, #4631, .T. ) ;
#2984 = CARTESIAN_POINT ( 'NONE',  ( -9.000000000000001776, 2.000000000000000000, -20.00000000000000000 ) ) ;
#2985 = FACE_OUTER_BOUND ( 'NONE', #4652, .T. ) ;
#2986 = CIRCLE ( 'NONE', #2426, 2.099999999999997868 ) ;
#2987 = VECTOR ( 'NONE', #3039, 1000.000000000000000 ) ;
#2988 = AXIS2_PLACEMENT_3D ( 'NONE', #845, #1250, #4622 ) ;
#2989 = DIRECTION ( 'NONE',  ( 0.000000000000000000, 0.000000000000000000, -1.000000000000000000 ) ) ;
#2990 = VERTEX_POINT ( 'NONE', #377 ) ;
#2991 = ADVANCED_FACE ( 'NONE', ( #3860 ), #403, .T. ) ;
#2992 = LINE ( 'NONE', #2611, #3691 ) ;
#2993 = CARTESIAN_POINT ( 'NONE',  ( 25.00000000000000000, 2.516649172247811061E-16, -2.055000000000000160 ) ) ;
#2994 = DIRECTION ( 'NONE',  ( 0.000000000000000000, 0.5000000000000011102, 0.8660254037844379305 ) ) ;
#2995 = AXIS2_PLACEMENT_3D ( 'NONE', #4848, #338, #4926 ) ;
#2996 = ORIENTED_EDGE ( 'NONE', *, *, #2555, .T. ) ;
#2997 = EDGE_CURVE ( 'NONE', #4073, #3915, #4256, .T. ) ;
#2998 = EDGE_CURVE ( 'NONE', #571, #115, #1961, .T. ) ;
#2999 = ORIENTED_EDGE ( 'NONE', *, *, #1396, .T. ) ;
#3000 = CARTESIAN_POINT ( 'NONE',  ( -7.332110811570578784E-14, -6.999999999999999112, -32.00000000000000000 ) ) ;
#3001 = DIRECTION ( 'NONE',  ( 2.168404344971009361E-16, -1.000000000000000000, 0.000000000000000000 ) ) ;
#3002 = LINE ( 'NONE', #3690, #2676 ) ;
#3003 = ORIENTED_EDGE ( 'NONE', *, *, #751, .T. ) ;
#3004 = ORIENTED_EDGE ( 'NONE', *, *, #2315, .F. ) ;
#3005 = FACE_OUTER_BOUND ( 'NONE', #4754, .T. ) ;
#3006 = DIRECTION ( 'NONE',  ( -1.000000000000000000, -0.000000000000000000, -0.000000000000000000 ) ) ;
#3007 = CARTESIAN_POINT ( 'NONE',  ( 0.000000000000000000, 0.000000000000000000, -4.000000000000000000 ) ) ;
#3008 = AXIS2_PLACEMENT_3D ( 'NONE', #1308, #4733, #1259 ) ;
#3009 = CARTESIAN_POINT ( 'NONE',  ( -6.537332342993324937E-14, 16.00000000000000000, -23.90000000000000568 ) ) ;
#3010 = ORIENTED_EDGE ( 'NONE', *, *, #3262, .T. ) ;
#3011 = FACE_OUTER_BOUND ( 'NONE', #2154, .T. ) ;
#3012 = ITEM_DEFINED_TRANSFORMATION ( 'NONE', 'NONE', #4215,  #1918 ) ;
#3013 = CARTESIAN_POINT ( 'NONE',  ( 0.000000000000000000, 0.000000000000000000, 4.000000000000000000 ) ) ;
#3014 = ORIENTED_EDGE ( 'NONE', *, *, #3941, .T. ) ;
#3015 = DIRECTION ( 'NONE',  ( 1.357798298438996130E-15, -1.000000000000000000, 0.000000000000000000 ) ) ;
#3016 = LINE ( 'NONE', #2632, #743 ) ;
#3017 = PLANE ( 'NONE',  #1696 ) ;
#3018 = LINE ( 'NONE', #4527, #1143 ) ;
#3019 = EDGE_CURVE ( 'NONE', #754, #1649, #2413, .T. ) ;
#3020 = ORIENTED_EDGE ( 'NONE', *, *, #2810, .T. ) ;
#3021 = ORIENTED_EDGE ( 'NONE', *, *, #1883, .F. ) ;
#3022 =( NAMED_UNIT ( * ) PLANE_ANGLE_UNIT ( ) SI_UNIT ( $, .RADIAN. ) );
#3023 = CARTESIAN_POINT ( 'NONE',  ( 0.000000000000000000, 0.000000000000000000, -20.00000000000000000 ) ) ;
#3024 = LINE ( 'NONE', #1138, #4746 ) ;
#3025 = CARTESIAN_POINT ( 'NONE',  ( 21.97815564317848924, -11.91494984865602902, -20.41093891521751047 ) ) ;
#3026 = ADVANCED_FACE ( 'NONE', ( #4610 ), #1523, .T. ) ;
#3027 = VERTEX_POINT ( 'NONE', #74 ) ;
#3028 = EDGE_LOOP ( 'NONE', ( #2049, #764, #2883, #4416, #4493 ) ) ;
#3029 = CARTESIAN_POINT ( 'NONE',  ( -12.50000000000000000, -1.383461737289380927E-15, 12.00000000000000000 ) ) ;
#3030 = DIRECTION ( 'NONE',  ( -1.000000000000000000, -0.000000000000000000, 0.000000000000000000 ) ) ;
#3031 = ADVANCED_FACE ( 'NONE', ( #3906, #4224 ), #3069, .F. ) ;
#3032 = EDGE_LOOP ( 'NONE', ( #491, #3733, #2857, #95 ) ) ;
#3033 = FACE_OUTER_BOUND ( 'NONE', #4283, .T. ) ;
#3034 = ORIENTED_EDGE ( 'NONE', *, *, #3675, .F. ) ;
#3035 = PRODUCT_DEFINITION_CONTEXT ( 'detailed design', #4189, 'design' ) ;
#3036 = CARTESIAN_POINT ( 'NONE',  ( 22.03949535914419755, 11.80087472665740300, -30.28571428571428470 ) ) ;
#3037 = DIRECTION ( 'NONE',  ( 1.000000000000000000, -0.000000000000000000, -0.000000000000000000 ) ) ;
#3038 = DIRECTION ( 'NONE',  ( 0.000000000000000000, -0.4999999999999993339, 0.8660254037844389297 ) ) ;
#3039 = DIRECTION ( 'NONE',  ( -1.000000000000000000, -0.000000000000000000, -0.000000000000000000 ) ) ;
#3040 = AXIS2_PLACEMENT_3D ( 'NONE', #1301, #123, #1344 ) ;
#3041 = ORIENTED_EDGE ( 'NONE', *, *, #628, .F. ) ;
#3042 = EDGE_CURVE ( 'NONE', #1050, #3389, #1526, .T. ) ;
#3043 = DIRECTION ( 'NONE',  ( 0.000000000000000000, 0.000000000000000000, -1.000000000000000000 ) ) ;
#3044 = VECTOR ( 'NONE', #1697, 1000.000000000000000 ) ;
#3045 = CARTESIAN_POINT ( 'NONE',  ( 0.000000000000000000, 0.000000000000000000, -20.00000000000000000 ) ) ;
#3046 = CARTESIAN_POINT ( 'NONE',  ( 25.00000000000000000, 2.055000000000000160, 0.000000000000000000 ) ) ;
#3047 = DIRECTION ( 'NONE',  ( 0.000000000000000000, 0.000000000000000000, -1.000000000000000000 ) ) ;
#3048 = ORIENTED_EDGE ( 'NONE', *, *, #2905, .F. ) ;
#3049 = VECTOR ( 'NONE', #4044, 1000.000000000000000 ) ;
#3050 = CARTESIAN_POINT ( 'NONE',  ( 2.500000000000000000, 0.000000000000000000, 0.000000000000000000 ) ) ;
#3051 = PRODUCT_RELATED_PRODUCT_CATEGORY ( 'part', '', ( #51 ) ) ;
#3052 = EDGE_CURVE ( 'NONE', #2206, #4462, #1981, .T. ) ;
#3053 = FACE_OUTER_BOUND ( 'NONE', #4928, .T. ) ;
#3054 = CARTESIAN_POINT ( 'NONE',  ( -25.00000000000000000, 3.061616997868383043E-15, -32.00000000000000000 ) ) ;
#3055 = CIRCLE ( 'NONE', #888, 2.099999999999997868 ) ;
#3056 = ORIENTED_EDGE ( 'NONE', *, *, #2492, .F. ) ;
#3057 = VECTOR ( 'NONE', #384, 1000.000000000000000 ) ;
#3058 = EDGE_CURVE ( 'NONE', #340, #1461, #857, .T. ) ;
#3059 = EDGE_CURVE ( 'NONE', #4410, #4395, #3509, .T. ) ;
#3060 = CARTESIAN_POINT ( 'NONE',  ( -6.517431832507181422E-14, 16.00000000000000000, -23.90000000000000568 ) ) ;
#3061 = EDGE_LOOP ( 'NONE', ( #4214, #143, #2461, #3886 ) ) ;
#3062 = AXIS2_PLACEMENT_3D ( 'NONE', #155, #1728, #4340 ) ;
#3063 = CIRCLE ( 'NONE', #6, 25.00000000000000000 ) ;
#3064 = ORIENTED_EDGE ( 'NONE', *, *, #3907, .F. ) ;
#3065 = VECTOR ( 'NONE', #2855, 1000.000000000000114 ) ;
#3066 = AXIS2_PLACEMENT_3D ( 'NONE', #935, #916, #2462 ) ;
#3067 = CARTESIAN_POINT ( 'NONE',  ( 22.88998946896871800, -10.05230818559221717, -26.81638557257617705 ) ) ;
#3068 = CARTESIAN_POINT ( 'NONE',  ( 2.500000000000000000, 1.768423874527824902, 1.020999999999999019 ) ) ;
#3069 = PLANE ( 'NONE',  #4249 ) ;
#3070 = CARTESIAN_POINT ( 'NONE',  ( 23.68543856465402442, 7.999999999999994671, -12.00000000000000000 ) ) ;
#3071 = VECTOR ( 'NONE', #3859, 1000.000000000000000 ) ;
#3072 = AXIS2_PLACEMENT_3D ( 'NONE', #1714, #4846, #4389 ) ;
#3073 = ORIENTED_EDGE ( 'NONE', *, *, #2803, .F. ) ;
#3074 = CARTESIAN_POINT ( 'NONE',  ( 0.000000000000000000, 0.000000000000000000, 2.000000000000001776 ) ) ;
#3075 = TOROIDAL_SURFACE ( 'NONE', #4341, 2.700000000000001066, 0.2000000000000000111 ) ;
#3076 = FACE_OUTER_BOUND ( 'NONE', #2519, .T. ) ;
#3077 = DIRECTION ( 'NONE',  ( 1.000000000000000000, -0.000000000000000000, -0.000000000000000000 ) ) ;
#3078 = FACE_BOUND ( 'NONE', #2109, .T. ) ;
#3079 = EDGE_LOOP ( 'NONE', ( #4632, #255, #2367, #2591 ) ) ;
#3080 = CIRCLE ( 'NONE', #3701, 2.099999999999997868 ) ;
#3081 = ORIENTED_EDGE ( 'NONE', *, *, #2378, .F. ) ;
#3082 =( NAMED_UNIT ( * ) SI_UNIT ( $, .STERADIAN. ) SOLID_ANGLE_UNIT ( ) );
#3083 = PLANE ( 'NONE',  #2490 ) ;
#3084 = DIRECTION ( 'NONE',  ( 0.000000000000000000, -0.4999999999999992784, 0.8660254037844389297 ) ) ;
#3085 = ORIENTED_EDGE ( 'NONE', *, *, #4424, .T. ) ;
#3086 = PLANE ( 'NONE',  #2339 ) ;
#3087 = TOROIDAL_SURFACE ( 'NONE', #3631, 4.000000000000000000, 0.2500000000000000000 ) ;
#3088 = DIRECTION ( 'NONE',  ( -0.000000000000000000, -0.000000000000000000, 1.000000000000000000 ) ) ;
#3089 = DIRECTION ( 'NONE',  ( 1.000000000000000000, -0.000000000000000000, -0.000000000000000000 ) ) ;
#3090 = ORIENTED_EDGE ( 'NONE', *, *, #3748, .T. ) ;
#3091 = ORIENTED_EDGE ( 'NONE', *, *, #2627, .T. ) ;
#3092 = CARTESIAN_POINT ( 'NONE',  ( -9.000000000000001776, 2.000000000000000000, -32.00000000000000000 ) ) ;
#3093 = DIRECTION ( 'NONE',  ( 0.000000000000000000, 0.000000000000000000, 1.000000000000000000 ) ) ;
#3094 = CARTESIAN_POINT ( 'NONE',  ( -31.74999999999995737, 5.204748896376250699E-16, -4.250000000000000000 ) ) ;
#3095 = CARTESIAN_POINT ( 'NONE',  ( -9.000000000000001776, 2.000000000000000000, -12.00000000000000000 ) ) ;
#3096 = ORIENTED_EDGE ( 'NONE', *, *, #2309, .T. ) ;
#3097 = PRODUCT_DEFINITION_SHAPE ( 'NONE', 'NONE',  #4361 ) ;
#3098 = CARTESIAN_POINT ( 'NONE',  ( 19.00000000000018474, -16.00000000000028066, -25.99999999999969802 ) ) ;
#3099 = DIRECTION ( 'NONE',  ( 0.000000000000000000, 0.000000000000000000, -1.000000000000000000 ) ) ;
#3100 = CARTESIAN_POINT ( 'NONE',  ( 25.00000000000000000, 0.000000000000000000, -1.999999999999994893 ) ) ;
#3101 = DIRECTION ( 'NONE',  ( -0.5000000000000061062, 1.060575238724902601E-16, -0.8660254037844351549 ) ) ;
#3102 = ORIENTED_EDGE ( 'NONE', *, *, #1935, .T. ) ;
#3103 = ORIENTED_EDGE ( 'NONE', *, *, #3540, .T. ) ;
#3104 = CARTESIAN_POINT ( 'NONE',  ( -2.042664716792774803E-14, 16.00000000000000000, -26.00000000000000355 ) ) ;
#3105 = DIRECTION ( 'NONE',  ( -1.000000000000000000, 0.000000000000000000, 0.000000000000000000 ) ) ;
#3106 = CARTESIAN_POINT ( 'NONE',  ( 2.500000000000000000, 1.178949249685213863, -2.042000000000001148 ) ) ;
#3107 = ORIENTED_EDGE ( 'NONE', *, *, #802, .T. ) ;
#3108 = DIRECTION ( 'NONE',  ( 0.000000000000000000, 0.000000000000000000, -1.000000000000000000 ) ) ;
#3109 = DIRECTION ( 'NONE',  ( 0.000000000000000000, 0.000000000000000000, -1.000000000000000000 ) ) ;
#3110 = EDGE_CURVE ( 'NONE', #2345, #4346, #490, .T. ) ;
#3111 = ORIENTED_EDGE ( 'NONE', *, *, #1095, .F. ) ;
#3112 = ORIENTED_EDGE ( 'NONE', *, *, #1060, .F. ) ;
#3113 = EDGE_CURVE ( 'NONE', #2206, #3948, #3535, .T. ) ;
#3114 = AXIS2_PLACEMENT_3D ( 'NONE', #4963, #4530, #409 ) ;
#3115 = CARTESIAN_POINT ( 'NONE',  ( 5.200000000000002842, 0.000000000000000000, 0.000000000000000000 ) ) ;
#3116 = DIRECTION ( 'NONE',  ( -0.000000000000000000, 1.471414886128461471E-15, 1.000000000000000000 ) ) ;
#3117 = ORIENTED_EDGE ( 'NONE', *, *, #2074, .T. ) ;
#3118 = ORIENTED_EDGE ( 'NONE', *, *, #966, .T. ) ;
#3119 = EDGE_CURVE ( 'NONE', #1989, #1050, #182, .T. ) ;
#3120 = CONTEXT_DEPENDENT_SHAPE_REPRESENTATION ( #3184, #131 ) ;
#3121 = CARTESIAN_POINT ( 'NONE',  ( 2.886521338340684917, 0.000000000000000000, 0.000000000000000000 ) ) ;
#3122 = DIRECTION ( 'NONE',  ( 0.000000000000000000, 0.000000000000000000, 1.000000000000000000 ) ) ;
#3123 = CARTESIAN_POINT ( 'NONE',  ( 22.40016391766193493, 11.10102051443364068, -32.00000000000000000 ) ) ;
#3124 = ORIENTED_EDGE ( 'NONE', *, *, #4220, .F. ) ;
#3125 = CIRCLE ( 'NONE', #242, 6.999999999999999112 ) ;
#3126 = VERTEX_POINT ( 'NONE', #3628 ) ;
#3127 = FILL_AREA_STYLE_COLOUR ( '', #4717 ) ;
#3128 = DIRECTION ( 'NONE',  ( 0.000000000000000000, 0.000000000000000000, -1.000000000000000000 ) ) ;
#3129 = CYLINDRICAL_SURFACE ( 'NONE', #906, 22.99999999999998934 ) ;
#3130 = LINE ( 'NONE', #3106, #1704 ) ;
#3131 = ORIENTED_EDGE ( 'NONE', *, *, #1669, .F. ) ;
#3132 = DIRECTION ( 'NONE',  ( -1.000000000000000000, 0.000000000000000000, 0.000000000000000000 ) ) ;
#3133 = LINE ( 'NONE', #3900, #2967 ) ;
#3134 = VECTOR ( 'NONE', #3256, 1000.000000000000000 ) ;
#3135 = EDGE_LOOP ( 'NONE', ( #4453, #2027, #2034, #2070, #2296, #2279 ) ) ;
#3136 = ORIENTED_EDGE ( 'NONE', *, *, #690, .F. ) ;
#3137 = AXIS2_PLACEMENT_3D ( 'NONE', #1908, #3788, #311 ) ;
#3138 = CARTESIAN_POINT ( 'NONE',  ( 22.89074894326664378, -10.05057747304974569, -25.19644245487525325 ) ) ;
#3139 = CARTESIAN_POINT ( 'NONE',  ( 2.000000000000000000, 0.000000000000000000, 0.000000000000000000 ) ) ;
#3140 = DIRECTION ( 'NONE',  ( 0.000000000000000000, 0.000000000000000000, -1.000000000000000000 ) ) ;
#3141 = ORIENTED_EDGE ( 'NONE', *, *, #11, .T. ) ;
#3142 = ADVANCED_FACE ( 'NONE', ( #3979 ), #2513, .T. ) ;
#3143 = ORIENTED_EDGE ( 'NONE', *, *, #4830, .T. ) ;
#3144 = VECTOR ( 'NONE', #4771, 1000.000000000000000 ) ;
#3145 = AXIS2_PLACEMENT_3D ( 'NONE', #207, #1727, #2139 ) ;
#3146 = PRODUCT_CONTEXT ( 'NONE', #4288, 'mechanical' ) ;
#3147 = CARTESIAN_POINT ( 'NONE',  ( 2.000000000000000000, -0.8865213383406690406, 1.535500000000000975 ) ) ;
#3148 = DIRECTION ( 'NONE',  ( 0.9474175425861609545, 0.3199999999999996181, 0.000000000000000000 ) ) ;
#3149 = CONICAL_SURFACE ( 'NONE', #3379, 2.055000000000000160, 0.7853981633974721488 ) ;
#3150 = CARTESIAN_POINT ( 'NONE',  ( -3.642919299551294898E-14, -16.00000000000000000, -26.00000000000000355 ) ) ;
#3151 = EDGE_CURVE ( 'NONE', #4738, #4892, #151, .T. ) ;
#3152 = EDGE_CURVE ( 'NONE', #1695, #4670, #1303, .T. ) ;
#3153 = EDGE_CURVE ( 'NONE', #1203, #4122, #910, .T. ) ;
#3154 = VERTEX_POINT ( 'NONE', #4418 ) ;
#3155 = VECTOR ( 'NONE', #2738, 1000.000000000000000 ) ;
#3156 = EDGE_LOOP ( 'NONE', ( #1231, #4041, #4588, #2848 ) ) ;
#3157 = SURFACE_STYLE_USAGE ( .BOTH. , #1614 ) ;
#3158 = DIRECTION ( 'NONE',  ( -1.000000000000000000, -0.000000000000000000, -0.000000000000000000 ) ) ;
#3159 = DIRECTION ( 'NONE',  ( -0.000000000000000000, -0.000000000000000000, 1.000000000000000000 ) ) ;
#3160 = DIRECTION ( 'NONE',  ( 0.000000000000000000, 0.000000000000000000, -1.000000000000000000 ) ) ;
#3161 = ORIENTED_EDGE ( 'NONE', *, *, #4704, .T. ) ;
#3162 = FACE_OUTER_BOUND ( 'NONE', #1225, .T. ) ;
#3163 = CLOSED_SHELL ( 'NONE', ( #4542, #3566, #3390, #622, #3597, #2714, #1420, #3958, #2777, #208, #2689, #386, #3241, #4075, #2160, #1725, #1485, #3768, #2438, #3205 ) ) ;
#3164 = DIRECTION ( 'NONE',  ( 0.000000000000000000, 0.000000000000000000, -1.000000000000000000 ) ) ;
#3165 = VERTEX_POINT ( 'NONE', #992 ) ;
#3166 = ORIENTED_EDGE ( 'NONE', *, *, #3451, .F. ) ;
#3167 = CIRCLE ( 'NONE', #2274, 25.00000000000000000 ) ;
#3168 = DIRECTION ( 'NONE',  ( 0.000000000000000000, 0.000000000000000000, -1.000000000000000000 ) ) ;
#3169 = VECTOR ( 'NONE', #554, 1000.000000000000114 ) ;
#3170 = DIRECTION ( 'NONE',  ( 0.000000000000000000, 0.000000000000000000, 1.000000000000000000 ) ) ;
#3171 = DIRECTION ( 'NONE',  ( -0.000000000000000000, -0.000000000000000000, -1.000000000000000000 ) ) ;
#3172 = ORIENTED_EDGE ( 'NONE', *, *, #1107, .F. ) ;
#3173 = ORIENTED_EDGE ( 'NONE', *, *, #2492, .T. ) ;
#3174 = CARTESIAN_POINT ( 'NONE',  ( 0.000000000000000000, 0.000000000000000000, -32.00000000000000000 ) ) ;
#3175 = EDGE_CURVE ( 'NONE', #1323, #1525, #2526, .T. ) ;
#3176 = DIRECTION ( 'NONE',  ( -0.5000000000000061062, 0.000000000000000000, 0.8660254037844351549 ) ) ;
#3177 = LINE ( 'NONE', #3634, #901 ) ;
#3178 = EDGE_LOOP ( 'NONE', ( #3612, #2628, #2095, #2910 ) ) ;
#3179 = ORIENTED_EDGE ( 'NONE', *, *, #3682, .T. ) ;
#3180 = CARTESIAN_POINT ( 'NONE',  ( -2.042664716792774803E-14, 16.00000000000000000, -23.90000000000001279 ) ) ;
#3181 = EDGE_CURVE ( 'NONE', #479, #2834, #2986, .T. ) ;
#3182 = DIRECTION ( 'NONE',  ( 4.073394895316987600E-15, -1.000000000000000000, 0.000000000000000000 ) ) ;
#3183 = ORIENTED_EDGE ( 'NONE', *, *, #2852, .T. ) ;
#3184 =( REPRESENTATION_RELATIONSHIP ('NONE','NONE', #137, #4221 ) REPRESENTATION_RELATIONSHIP_WITH_TRANSFORMATION ( #2368 )SHAPE_REPRESENTATION_RELATIONSHIP( ) );
#3185 = LINE ( 'NONE', #4726, #4470 ) ;
#3186 = EDGE_CURVE ( 'Edge1', #4063, #2762, #1699, .T. ) ;
#3187 = DIRECTION ( 'NONE',  ( -1.000000000000000000, 0.000000000000000000, 0.000000000000000000 ) ) ;
#3188 = ORIENTED_EDGE ( 'NONE', *, *, #1884, .T. ) ;
#3189 = DIRECTION ( 'NONE',  ( 0.000000000000000000, 0.4999999999999993894, -0.8660254037844389297 ) ) ;
#3190 = ORIENTED_EDGE ( 'NONE', *, *, #4855, .T. ) ;
#3191 = ORIENTED_EDGE ( 'NONE', *, *, #2204, .F. ) ;
#3192 = CARTESIAN_POINT ( 'NONE',  ( 0.000000000000000000, 0.000000000000000000, -20.00000000000000000 ) ) ;
#3193 = DIRECTION ( 'NONE',  ( 1.000000000000000000, 0.000000000000000000, 0.000000000000000000 ) ) ;
#3194 = LINE ( 'NONE', #1318, #3065 ) ;
#3195 = ORIENTED_EDGE ( 'NONE', *, *, #684, .F. ) ;
#3196 = EDGE_CURVE ( 'NONE', #4670, #1695, #651, .T. ) ;
#3197 = ORIENTED_EDGE ( 'NONE', *, *, #1155, .F. ) ;
#3198 = DIRECTION ( 'NONE',  ( 0.000000000000000000, 0.000000000000000000, -1.000000000000000000 ) ) ;
#3199 = PRODUCT_DEFINITION_FORMATION_WITH_SPECIFIED_SOURCE ( 'ANY', '', #263, .NOT_KNOWN. ) ;
#3200 = FACE_OUTER_BOUND ( 'NONE', #1702, .T. ) ;
#3201 = CARTESIAN_POINT ( 'NONE',  ( 25.00000000000000000, 3.061616997868383043E-15, -1.999999999999994893 ) ) ;
#3202 = ORIENTED_EDGE ( 'NONE', *, *, #1910, .T. ) ;
#3203 = VECTOR ( 'NONE', #4699, 1000.000000000000114 ) ;
#3204 = ADVANCED_FACE ( 'NONE', ( #1761 ), #3149, .T. ) ;
#3205 = ADVANCED_FACE ( 'NONE', ( #2128 ), #1737, .F. ) ;
#3206 = CYLINDRICAL_SURFACE ( 'NONE', #2964, 25.00000000000000000 ) ;
#3207 = LINE ( 'NONE', #2381, #4155 ) ;
#3208 = AXIS2_PLACEMENT_3D ( 'NONE', #217, #1794, #4852 ) ;
#3209 = VERTEX_POINT ( 'NONE', #2055 ) ;
#3210 = ADVANCED_FACE ( 'NONE', ( #1015 ), #2545, .T. ) ;
#3211 = EDGE_CURVE ( 'NONE', #1968, #1680, #3455, .T. ) ;
#3212 = AXIS2_PLACEMENT_3D ( 'NONE', #4300, #3881, #3164 ) ;
#3213 = DIRECTION ( 'NONE',  ( 0.5150380749100550437, 0.000000000000000000, -0.8571673007021117785 ) ) ;
#3214 = DIRECTION ( 'NONE',  ( -1.000000000000000000, 0.000000000000000000, 0.000000000000000000 ) ) ;
#3215 = DIRECTION ( 'NONE',  ( 0.000000000000000000, 0.000000000000000000, -1.000000000000000000 ) ) ;
#3216 = AXIS2_PLACEMENT_3D ( 'NONE', #2350, #2877, #632 ) ;
#3217 = VERTEX_POINT ( 'NONE', #1069 ) ;
#3218 = ORIENTED_EDGE ( 'NONE', *, *, #1745, .T. ) ;
#3219 = AXIS2_PLACEMENT_3D ( 'NONE', #1756, #2494, #588 ) ;
#3220 = CIRCLE ( 'NONE', #4567, 22.99999999999998934 ) ;
#3221 = FACE_OUTER_BOUND ( 'NONE', #1354, .T. ) ;
#3222 = LINE ( 'NONE', #3655, #2743 ) ;
#3223 = DIRECTION ( 'NONE',  ( -0.3199999999999996736, 0.9474175425861610655, 0.000000000000000000 ) ) ;
#3224 = VECTOR ( 'NONE', #3171, 1000.000000000000000 ) ;
#3225 = ORIENTED_EDGE ( 'NONE', *, *, #362, .F. ) ;
#3226 = ORIENTED_EDGE ( 'NONE', *, *, #146, .T. ) ;
#3227 = DIRECTION ( 'NONE',  ( 0.000000000000000000, 0.4999999999999990008, -0.8660254037844391517 ) ) ;
#3228 = STYLED_ITEM ( 'NONE', ( #4307 ), #2009 ) ;
#3229 = CARTESIAN_POINT ( 'NONE',  ( 21.90877321452243010, 12.04191644460182609, -21.39663540706808575 ) ) ;
#3230 = LINE ( 'NONE', #590, #2354 ) ;
#3231 = ORIENTED_EDGE ( 'NONE', *, *, #322, .F. ) ;
#3232 = VECTOR ( 'NONE', #1598, 1000.000000000000000 ) ;
#3233 = AXIS2_PLACEMENT_3D ( 'NONE', #4135, #3414, #1064 ) ;
#3234 = DIRECTION ( 'NONE',  ( 0.000000000000000000, 0.000000000000000000, 1.000000000000000000 ) ) ;
#3235 = CARTESIAN_POINT ( 'NONE',  ( -25.00000000000000000, 0.000000000000000000, 2.000000000000001776 ) ) ;
#3236 = CIRCLE ( 'NONE', #4422, 25.00000000000000000 ) ;
#3237 = ORIENTED_EDGE ( 'NONE', *, *, #715, .F. ) ;
#3238 = PRODUCT_DEFINITION_CONTEXT ( 'detailed design', #1377, 'design' ) ;
#3239 = PLANE ( 'NONE',  #4111 ) ;
#3240 = DIRECTION ( 'NONE',  ( 1.000000000000000000, 0.000000000000000000, 0.000000000000000000 ) ) ;
#3241 = ADVANCED_FACE ( 'NONE', ( #1432 ), #1092, .F. ) ;
#3242 = AXIS2_PLACEMENT_3D ( 'NONE', #1675, #1135, #3435 ) ;
#3243 = EDGE_LOOP ( 'NONE', ( #2292, #1975, #2407, #1391 ) ) ;
#3244 = ORIENTED_EDGE ( 'NONE', *, *, #4825, .F. ) ;
#3245 = CIRCLE ( 'NONE', #3877, 2.200000000000001066 ) ;
#3246 = CARTESIAN_POINT ( 'NONE',  ( -3.642919299551294898E-14, 16.00000000000000000, -28.64999999999999858 ) ) ;
#3247 = EDGE_CURVE ( 'NONE', #4690, #2692, #2660, .T. ) ;
#3248 = FACE_OUTER_BOUND ( 'NONE', #1020, .T. ) ;
#3249 = DIRECTION ( 'NONE',  ( 0.000000000000000000, -0.5000000000000011102, -0.8660254037844379305 ) ) ;
#3250 = ORIENTED_EDGE ( 'NONE', *, *, #1877, .F. ) ;
#3251 = CYLINDRICAL_SURFACE ( 'NONE', #728, 23.00000000000000711 ) ;
#3252 = CARTESIAN_POINT ( 'NONE',  ( 21.37171027316252747, 8.499999999999930722, -12.00000000000000000 ) ) ;
#3253 = EDGE_LOOP ( 'NONE', ( #2293, #1363, #663, #4818 ) ) ;
#3254 = DIRECTION ( 'NONE',  ( 0.000000000000000000, 0.000000000000000000, 1.000000000000000000 ) ) ;
#3255 = CARTESIAN_POINT ( 'NONE',  ( 0.000000000000000000, 0.000000000000000000, -32.00000000000000000 ) ) ;
#3256 = DIRECTION ( 'NONE',  ( -1.000000000000000000, -0.000000000000000000, -0.000000000000000000 ) ) ;
#3257 = ORIENTED_EDGE ( 'NONE', *, *, #1544, .T. ) ;
#3258 = EDGE_CURVE ( 'NONE', #4802, #894, #3696, .T. ) ;
#3259 = CONTEXT_DEPENDENT_SHAPE_REPRESENTATION ( #4612, #2779 ) ;
#3260 = DIRECTION ( 'NONE',  ( 0.000000000000000000, 0.000000000000000000, -1.000000000000000000 ) ) ;
#3261 = VERTEX_POINT ( 'NONE', #4901 ) ;
#3262 = EDGE_CURVE ( 'NONE', #3494, #4690, #4740, .T. ) ;
#3263 = CARTESIAN_POINT ( 'NONE',  ( -25.00000000000000000, 0.000000000000000000, -1.999999999999994893 ) ) ;
#3264 = DIRECTION ( 'NONE',  ( 1.000000000000000000, 0.000000000000000000, 0.000000000000000000 ) ) ;
#3265 = FACE_OUTER_BOUND ( 'NONE', #1163, .T. ) ;
#3266 = ORIENTED_EDGE ( 'NONE', *, *, #1333, .F. ) ;
#3267 = EDGE_CURVE ( 'NONE', #7, #519, #2241, .T. ) ;
#3268 = PRESENTATION_LAYER_ASSIGNMENT (  '', '', ( #478 ) ) ;
#3269 = EDGE_CURVE ( 'NONE', #484, #4568, #341, .T. ) ;
#3270 = ORIENTED_EDGE ( 'NONE', *, *, #2010, .F. ) ;
#3271 = CARTESIAN_POINT ( 'NONE',  ( 5.000000000000004441, 0.000000000000000000, 0.000000000000000000 ) ) ;
#3272 = DIRECTION ( 'NONE',  ( -0.000000000000000000, -0.000000000000000000, 1.000000000000000000 ) ) ;
#3273 = DIRECTION ( 'NONE',  ( -1.000000000000000000, 3.357200482488896896E-15, 0.000000000000000000 ) ) ;
#3274 = EDGE_LOOP ( 'NONE', ( #4910, #2818, #3103, #2075 ) ) ;
#3275 = DIRECTION ( 'NONE',  ( -1.000000000000000000, 0.000000000000000000, 0.000000000000000000 ) ) ;
#3276 = CARTESIAN_POINT ( 'NONE',  ( 22.40016391766193493, -11.10102051443364068, -32.00000000000000000 ) ) ;
#3277 = ORIENTED_EDGE ( 'NONE', *, *, #2379, .T. ) ;
#3278 = DIRECTION ( 'NONE',  ( 0.000000000000000000, -1.000000000000000000, 9.783878858594330870E-16 ) ) ;
#3279 = VECTOR ( 'NONE', #2763, 1000.000000000000000 ) ;
#3280 = CARTESIAN_POINT ( 'NONE',  ( 0.000000000000000000, 0.000000000000000000, -12.00000000000000000 ) ) ;
#3281 =( NAMED_UNIT ( * ) PLANE_ANGLE_UNIT ( ) SI_UNIT ( $, .RADIAN. ) );
#3282 = EDGE_LOOP ( 'NONE', ( #287, #3021, #2453, #1156 ) ) ;
#3283 = FACE_OUTER_BOUND ( 'NONE', #3178, .T. ) ;
#3284 = VECTOR ( 'NONE', #2243, 1000.000000000000000 ) ;
#3285 = DIRECTION ( 'NONE',  ( -4.336808689942018722E-16, -1.000000000000000000, 0.000000000000000000 ) ) ;
#3286 = CARTESIAN_POINT ( 'NONE',  ( 25.00000000000000000, 3.061616997868383043E-15, 4.000000000000000000 ) ) ;
#3287 = ORIENTED_EDGE ( 'NONE', *, *, #1673, .T. ) ;
#3288 = AXIS2_PLACEMENT_3D ( 'NONE', #1293, #2469, #194 ) ;
#3289 = ORIENTED_EDGE ( 'NONE', *, *, #1176, .F. ) ;
#3290 = DIRECTION ( 'NONE',  ( 0.000000000000000000, 0.000000000000000000, 1.000000000000000000 ) ) ;
#3291 = CARTESIAN_POINT ( 'NONE',  ( 0.1999999999999987899, 0.000000000000000000, 3.500000000000000000 ) ) ;
#3292 = CARTESIAN_POINT ( 'NONE',  ( 21.96482728828171460, 11.94032596560094817, -21.57765196252147177 ) ) ;
#3293 = CONICAL_SURFACE ( 'NONE', #3933, 2.041999999999999815, 1.047197551196591858 ) ;
#3294 = CYLINDRICAL_SURFACE ( 'NONE', #4103, 2.099999999999997868 ) ;
#3295 = EDGE_CURVE ( 'NONE', #1595, #392, #4118, .T. ) ;
#3296 = CIRCLE ( 'NONE', #3605, 0.2000000000000000944 ) ;
#3297 = EDGE_CURVE ( 'NONE', #3361, #4023, #4252, .T. ) ;
#3298 = ORIENTED_EDGE ( 'NONE', *, *, #2659, .F. ) ;
#3299 = AXIS2_PLACEMENT_3D ( 'NONE', #314, #4929, #3325 ) ;
#3300 = COLOUR_RGB ( '', 0.66274510, 0.83137255, 0.94901961) ;
#3301 = CARTESIAN_POINT ( 'NONE',  ( -2.172477277502393807E-14, 16.00000000000000000, -26.00000000000000355 ) ) ;
#3302 = FACE_OUTER_BOUND ( 'NONE', #4865, .T. ) ;
#3303 = DIRECTION ( 'NONE',  ( -1.106769389831504313E-16, -1.000000000000000000, 0.000000000000000000 ) ) ;
#3304 = ADVANCED_FACE ( 'NONE', ( #344 ), #1412, .F. ) ;
#3305 = EDGE_CURVE ( 'NONE', #2431, #4296, #2107, .T. ) ;
#3306 = AXIS2_PLACEMENT_3D ( 'NONE', #2190, #260, #307 ) ;
#3307 = ORIENTED_EDGE ( 'NONE', *, *, #323, .F. ) ;
#3308 = CYLINDRICAL_SURFACE ( 'NONE', #1593, 2.099999999999994316 ) ;
#3309 = AXIS2_PLACEMENT_3D ( 'NONE', #696, #3746, #2353 ) ;
#3310 = DIRECTION ( 'NONE',  ( -1.000000000000000000, -0.000000000000000000, -0.000000000000000000 ) ) ;
#3311 = ORIENTED_EDGE ( 'NONE', *, *, #2502, .F. ) ;
#3312 = CARTESIAN_POINT ( 'NONE',  ( 0.2500000000000002220, 0.000000000000000000, 4.000000000000000000 ) ) ;
#3313 = CARTESIAN_POINT ( 'NONE',  ( 5.200000000000002842, 0.000000000000000000, 0.000000000000000000 ) ) ;
#3314 = DIRECTION ( 'NONE',  ( -1.000000000000000000, -0.000000000000000000, -0.000000000000000000 ) ) ;
#3315 = VERTEX_POINT ( 'NONE', #4464 ) ;
#3316 = VECTOR ( 'NONE', #3831, 1000.000000000000000 ) ;
#3317 = ORIENTED_EDGE ( 'NONE', *, *, #2204, .T. ) ;
#3318 = EDGE_CURVE ( 'NONE', #4311, #1059, #667, .T. ) ;
#3319 = CARTESIAN_POINT ( 'NONE',  ( -22.99999999999998934, 2.939152317953647894E-15, -4.000000000000000000 ) ) ;
#3320 = CARTESIAN_POINT ( 'NONE',  ( 12.50000000000000000, -1.383461737289380927E-15, 4.000000000000000000 ) ) ;
#3321 = VERTEX_POINT ( 'NONE', #3739 ) ;
#3322 = CARTESIAN_POINT ( 'NONE',  ( 0.000000000000000000, 25.00000000000000000, -20.00000000000000000 ) ) ;
#3323 = ORIENTED_EDGE ( 'NONE', *, *, #913, .F. ) ;
#3324 = ORIENTED_EDGE ( 'NONE', *, *, #1724, .F. ) ;
#3325 = DIRECTION ( 'NONE',  ( -1.000000000000000000, 0.000000000000000000, 0.000000000000000000 ) ) ;
#3326 = DIRECTION ( 'NONE',  ( -1.000000000000000000, 0.000000000000000000, 0.000000000000000000 ) ) ;
#3327 = DIRECTION ( 'NONE',  ( -1.000000000000000000, -0.000000000000000000, -0.000000000000000000 ) ) ;
#3328 = ORIENTED_EDGE ( 'NONE', *, *, #1162, .T. ) ;
#3329 = ADVANCED_FACE ( 'NONE', ( #293 ), #4899, .T. ) ;
#3330 = FACE_OUTER_BOUND ( 'NONE', #1766, .T. ) ;
#3331 = CARTESIAN_POINT ( 'NONE',  ( 0.000000000000000000, 0.000000000000000000, -4.000000000000000000 ) ) ;
#3332 = CARTESIAN_POINT ( 'NONE',  ( -14.00000000000006395, 16.00000000000000000, -28.10000000000000142 ) ) ;
#3333 = ORIENTED_EDGE ( 'NONE', *, *, #4943, .F. ) ;
#3334 = APPLICATION_CONTEXT ( 'automotive_design' ) ;
#3335 = FACE_OUTER_BOUND ( 'NONE', #3820, .T. ) ;
#3336 = DIRECTION ( 'NONE',  ( 0.000000000000000000, 0.000000000000000000, 1.000000000000000000 ) ) ;
#3337 = DIRECTION ( 'NONE',  ( 0.5150380749100544886, 1.049727191138618449E-16, 0.8571673007021121116 ) ) ;
#3338 = EDGE_LOOP ( 'NONE', ( #1586, #533, #2508, #3064 ) ) ;
#3339 = SHAPE_REPRESENTATION_RELATIONSHIP ( 'NONE' , 'NONE' ,  #3720, #469 ) ;
#3340 = FACE_OUTER_BOUND ( 'NONE', #4944, .T. ) ;
#3341 = CARTESIAN_POINT ( 'NONE',  ( 0.000000000000000000, -25.00000000000000000, -32.00000000000000000 ) ) ;
#3342 = DIRECTION ( 'NONE',  ( -1.000000000000000000, 0.000000000000000000, 0.000000000000000000 ) ) ;
#3343 = EDGE_CURVE ( 'NONE', #1024, #3700, #688, .T. ) ;
#3344 = ORIENTED_EDGE ( 'NONE', *, *, #820, .T. ) ;
#3345 = CARTESIAN_POINT ( 'NONE',  ( 0.000000000000000000, 0.000000000000000000, -12.00000000000000000 ) ) ;
#3346 = CARTESIAN_POINT ( 'NONE',  ( 25.00000000000000000, -16.00000000000000000, -26.00000000000000355 ) ) ;
#3347 = DIRECTION ( 'NONE',  ( 0.000000000000000000, 1.000000000000000000, -1.471414886128461471E-15 ) ) ;
#3348 = ORIENTED_EDGE ( 'NONE', *, *, #2167, .T. ) ;
#3349 = ADVANCED_FACE ( 'NONE', ( #636, #1145 ), #1835, .F. ) ;
#3350 = LINE ( 'NONE', #2984, #1749 ) ;
#3351 = SURFACE_SIDE_STYLE ('',( #353 ) ) ;
#3352 = CONTEXT_DEPENDENT_SHAPE_REPRESENTATION ( #3676, #2647 ) ;
#3353 = DIRECTION ( 'NONE',  ( -1.000000000000000000, -0.000000000000000000, -0.000000000000000000 ) ) ;
#3354 = EDGE_CURVE ( 'NONE', #2765, #451, #4013, .T. ) ;
#3355 = EDGE_CURVE ( 'NONE', #4459, #4073, #2975, .T. ) ;
#3356 = ORIENTED_EDGE ( 'NONE', *, *, #601, .T. ) ;
#3357 = AXIS2_PLACEMENT_3D ( 'NONE', #824, #2297, #3818 ) ;
#3358 = FACE_OUTER_BOUND ( 'NONE', #828, .T. ) ;
#3359 = CARTESIAN_POINT ( 'NONE',  ( 0.000000000000000000, 0.000000000000000000, -32.00000000000000000 ) ) ;
#3360 = AXIS2_PLACEMENT_3D ( 'NONE', #1070, #993, #614 ) ;
#3361 = VERTEX_POINT ( 'NONE', #1900 ) ;
#3362 = VECTOR ( 'NONE', #3303, 1000.000000000000000 ) ;
#3363 = VERTEX_POINT ( 'NONE', #4200 ) ;
#3364 = DIRECTION ( 'NONE',  ( 0.000000000000000000, 0.000000000000000000, -1.000000000000000000 ) ) ;
#3365 = DIRECTION ( 'NONE',  ( 0.000000000000000000, -0.5000000000000012212, -0.8660254037844380415 ) ) ;
#3366 = CARTESIAN_POINT ( 'NONE',  ( 6.517431832507181422E-14, -16.00000000000000000, -26.00000000000000355 ) ) ;
#3367 = ORIENTED_EDGE ( 'NONE', *, *, #3152, .F. ) ;
#3368 = CARTESIAN_POINT ( 'NONE',  ( 0.000000000000000000, -25.00000000000000000, -32.00000000000000000 ) ) ;
#3369 = CARTESIAN_POINT ( 'NONE',  ( 15.00000000000000000, 16.00000000000000000, -26.00000000000000355 ) ) ;
#3370 = AXIS2_PLACEMENT_3D ( 'NONE', #780, #2420, #1561 ) ;
#3371 = CARTESIAN_POINT ( 'NONE',  ( 2.500000000000000000, -1.178949249685213863, 2.042000000000002924 ) ) ;
#3372 = AXIS2_PLACEMENT_3D ( 'NONE', #4558, #364, #1886 ) ;
#3373 = DIRECTION ( 'NONE',  ( -0.000000000000000000, -0.000000000000000000, 1.000000000000000000 ) ) ;
#3374 = EDGE_LOOP ( 'NONE', ( #883, #3225, #66, #2478, #1290, #1252 ) ) ;
#3375 = CIRCLE ( 'NONE', #2024, 2.099999999999997868 ) ;
#3376 = DIRECTION ( 'NONE',  ( 1.000000000000000000, -0.000000000000000000, -0.000000000000000000 ) ) ;
#3377 = DIRECTION ( 'NONE',  ( 1.000000000000000000, -0.000000000000000000, -0.000000000000000000 ) ) ;
#3378 = ADVANCED_FACE ( 'NONE', ( #699, #3386 ), #376, .F. ) ;
#3379 = AXIS2_PLACEMENT_3D ( 'NONE', #3620, #592, #3254 ) ;
#3380 = CONICAL_SURFACE ( 'NONE', #2988, 23.00000000000000711, 0.7853981633974473908 ) ;
#3381 = LINE ( 'NONE', #2725, #4828 ) ;
#3382 = ORIENTED_EDGE ( 'NONE', *, *, #4724, .T. ) ;
#3383 = VECTOR ( 'NONE', #2005, 1000.000000000000000 ) ;
#3384 = ADVANCED_FACE ( 'NONE', ( #3430 ), #438, .F. ) ;
#3385 = LINE ( 'NONE', #4939, #2181 ) ;
#3386 = FACE_OUTER_BOUND ( 'NONE', #4498, .T. ) ;
#3387 = DIRECTION ( 'NONE',  ( -1.000000000000000000, -0.000000000000000000, -0.000000000000000000 ) ) ;
#3388 = CARTESIAN_POINT ( 'NONE',  ( 21.37171027316252747, 8.499999999999930722, -4.000000000000000000 ) ) ;
#3389 = VERTEX_POINT ( 'NONE', #3068 ) ;
#3390 = ADVANCED_FACE ( 'NONE', ( #2710 ), #1183, .F. ) ;
#3391 = DIRECTION ( 'NONE',  ( 1.000000000000000000, 0.000000000000000000, 0.000000000000000000 ) ) ;
#3392 = FACE_OUTER_BOUND ( 'NONE', #1760, .T. ) ;
#3393 = CARTESIAN_POINT ( 'NONE',  ( 0.000000000000000000, -25.00000000000000000, -20.00000000000000000 ) ) ;
#3394 = DIRECTION ( 'NONE',  ( 0.000000000000000000, 0.000000000000000000, -1.000000000000000000 ) ) ;
#3395 = ORIENTED_EDGE ( 'NONE', *, *, #2437, .F. ) ;
#3396 = VERTEX_POINT ( 'NONE', #723 ) ;
#3397 = DIRECTION ( 'NONE',  ( 0.000000000000000000, 0.000000000000000000, 1.000000000000000000 ) ) ;
#3398 = CIRCLE ( 'NONE', #2603, 23.00000000000000711 ) ;
#3399 = CARTESIAN_POINT ( 'NONE',  ( 25.00000000000000000, 11.80087472665741011, -21.71428571428571530 ) ) ;
#3400 = CARTESIAN_POINT ( 'NONE',  ( 0.000000000000000000, 0.000000000000000000, -4.000000000000000000 ) ) ;
#3401 = VERTEX_POINT ( 'NONE', #2231 ) ;
#3402 = UNCERTAINTY_MEASURE_WITH_UNIT (LENGTH_MEASURE( 1.000000000000000082E-05 ), #4707, 'distance_accuracy_value', 'NONE');
#3403 = DIRECTION ( 'NONE',  ( -1.000000000000000000, 0.000000000000000000, 0.000000000000000000 ) ) ;
#3404 = CARTESIAN_POINT ( 'NONE',  ( -7.332110811570578784E-14, -6.999999999999999112, -32.00000000000000000 ) ) ;
#3405 = ORIENTED_EDGE ( 'NONE', *, *, #2998, .F. ) ;
#3406 = CARTESIAN_POINT ( 'NONE',  ( 6.999999999999999112, 0.000000000000000000, -20.00000000000000000 ) ) ;
#3407 = LINE ( 'NONE', #2612, #1532 ) ;
#3408 = LINE ( 'NONE', #1103, #2655 ) ;
#3409 = DIRECTION ( 'NONE',  ( 0.9474175425861605104, -0.3200000000000010059, 0.000000000000000000 ) ) ;
#3410 = VERTEX_POINT ( 'NONE', #1929 ) ;
#3411 = EDGE_CURVE ( 'NONE', #4618, #9, #2302, .T. ) ;
#3412 = CARTESIAN_POINT ( 'NONE',  ( -4.255825541081811095E-15, 1.860062294479941650E-16, 51.99999999999999289 ) ) ;
#3413 = FACE_OUTER_BOUND ( 'NONE', #1008, .T. ) ;
#3414 = DIRECTION ( 'NONE',  ( 0.000000000000000000, 1.000000000000000000, -1.224646799147353207E-16 ) ) ;
#3415 = CARTESIAN_POINT ( 'NONE',  ( 22.03949535914419755, 11.80087472665740300, -30.28571428571428470 ) ) ;
#3416 = EDGE_CURVE ( 'NONE', #4259, #852, #100, .T. ) ;
#3417 = EDGE_CURVE ( 'NONE', #1320, #1044, #3407, .T. ) ;
#3418 = ORIENTED_EDGE ( 'NONE', *, *, #4481, .T. ) ;
#3419 = DIRECTION ( 'NONE',  ( 1.106769389831504682E-16, -1.000000000000000000, 0.000000000000000000 ) ) ;
#3420 =( LENGTH_UNIT ( ) NAMED_UNIT ( * ) SI_UNIT ( .MILLI., .METRE. ) );
#3421 = CARTESIAN_POINT ( 'NONE',  ( -8.500000000000001776, -9.407539813567788568E-16, 4.000000000000000000 ) ) ;
#3422 = PRESENTATION_STYLE_ASSIGNMENT (( #1868 ) ) ;
#3423 = STYLED_ITEM ( 'NONE', ( #3918 ), #469 ) ;
#3424 = ORIENTED_EDGE ( 'NONE', *, *, #1027, .F. ) ;
#3425 = DIRECTION ( 'NONE',  ( 1.000000000000000000, 0.000000000000000000, -0.000000000000000000 ) ) ;
#3426 = LINE ( 'NONE', #3404, #3839 ) ;
#3427 = ORIENTED_EDGE ( 'NONE', *, *, #2278, .F. ) ;
#3428 = EDGE_LOOP ( 'NONE', ( #2069, #1477, #621, #2179, #1268 ) ) ;
#3429 = CARTESIAN_POINT ( 'NONE',  ( 22.65824501284922476, -10.56463292904779827, -28.54887252943416343 ) ) ;
#3430 = FACE_OUTER_BOUND ( 'NONE', #2122, .T. ) ;
#3431 = CARTESIAN_POINT ( 'NONE',  ( -25.00000000000000000, 0.000000000000000000, 4.000000000000000000 ) ) ;
#3432 = DIRECTION ( 'NONE',  ( -1.106769389831504189E-16, 1.000000000000000000, 0.000000000000000000 ) ) ;
#3433 = AXIS2_PLACEMENT_3D ( 'NONE', #4374, #1647, #2881 ) ;
#3434 = EDGE_LOOP ( 'NONE', ( #4162, #3442, #1859 ) ) ;
#3435 = DIRECTION ( 'NONE',  ( 0.000000000000000000, 1.000000000000000000, -1.287488025362403787E-15 ) ) ;
#3436 = SHAPE_REPRESENTATION_RELATIONSHIP ( 'NONE' , 'NONE' ,  #1326, #1407 ) ;
#3437 = DIRECTION ( 'NONE',  ( -1.000000000000000000, -0.000000000000000000, -0.000000000000000000 ) ) ;
#3438 = DIRECTION ( 'NONE',  ( 1.000000000000000000, 0.000000000000000000, 0.000000000000000000 ) ) ;
#3439 = CARTESIAN_POINT ( 'NONE',  ( 21.90822715901080642, 12.04290832652441168, -30.60487698215225194 ) ) ;
#3440 = ORIENTED_EDGE ( 'NONE', *, *, #1784, .F. ) ;
#3441 = AXIS2_PLACEMENT_3D ( 'NONE', #2327, #4626, #899 ) ;
#3442 = ORIENTED_EDGE ( 'NONE', *, *, #2137, .F. ) ;
#3443 = CARTESIAN_POINT ( 'NONE',  ( 25.00000000000000000, 0.000000000000000000, -12.00000000000000000 ) ) ;
#3444 = ADVANCED_FACE ( 'NONE', ( #2282 ), #4551, .T. ) ;
#3445 = LINE ( 'NONE', #15, #1701 ) ;
#3446 = AXIS2_PLACEMENT_3D ( 'NONE', #3104, #844, #4269 ) ;
#3447 = ORIENTED_EDGE ( 'NONE', *, *, #1061, .T. ) ;
#3448 = AXIS2_PLACEMENT_3D ( 'NONE', #2566, #1812, #2596 ) ;
#3449 = AXIS2_PLACEMENT_3D ( 'NONE', #4457, #3759, #2217 ) ;
#3450 = CARTESIAN_POINT ( 'NONE',  ( 15.00000000000000000, -11.80087472665740300, -30.28571428571428470 ) ) ;
#3451 = EDGE_CURVE ( 'NONE', #3209, #2856, #3824, .T. ) ;
#3452 = ORIENTED_EDGE ( 'NONE', *, *, #2276, .T. ) ;
#3453 = TOROIDAL_SURFACE ( 'NONE', #734, 3.299999999999999822, 0.2000000000000000111 ) ;
#3454 = ORIENTED_EDGE ( 'NONE', *, *, #1536, .T. ) ;
#3455 = CIRCLE ( 'NONE', #3299, 25.00000000000000000 ) ;
#3456 = CARTESIAN_POINT ( 'NONE',  ( 22.90859662698202825, 10.00982993400316978, -26.39899337456353123 ) ) ;
#3457 = CARTESIAN_POINT ( 'NONE',  ( -19.30673457630785350, -12.49999999999993250, -12.00000000000000000 ) ) ;
#3458 = CARTESIAN_POINT ( 'NONE',  ( 2.500000000000000000, 1.178949249685213863, -2.042000000000001148 ) ) ;
#3459 = AXIS2_PLACEMENT_3D ( 'NONE', #4736, #4708, #1282 ) ;
#3460 = AXIS2_PLACEMENT_3D ( 'NONE', #1341, #238, #962 ) ;
#3461 = ORIENTED_EDGE ( 'NONE', *, *, #4081, .F. ) ;
#3462 = LINE ( 'NONE', #1634, #506 ) ;
#3463 = DIRECTION ( 'NONE',  ( 0.5150380749100550437, 1.049727191138617956E-16, 0.8571673007021117785 ) ) ;
#3464 = CARTESIAN_POINT ( 'NONE',  ( 0.000000000000000000, 25.00000000000000000, -32.00000000000000000 ) ) ;
#3465 = ORIENTED_EDGE ( 'NONE', *, *, #1120, .F. ) ;
#3466 = CIRCLE ( 'NONE', #2506, 17.00000000000000000 ) ;
#3467 = ADVANCED_FACE ( 'NONE', ( #26 ), #1555, .T. ) ;
#3468 = EDGE_CURVE ( 'NONE', #1716, #3747, #348, .T. ) ;
#3469 = ORIENTED_EDGE ( 'NONE', *, *, #2137, .T. ) ;
#3470 =( LENGTH_UNIT ( ) NAMED_UNIT ( * ) SI_UNIT ( .MILLI., .METRE. ) );
#3471 = DIRECTION ( 'NONE',  ( 0.000000000000000000, 0.000000000000000000, 1.000000000000000000 ) ) ;
#3472 = LINE ( 'NONE', #3920, #4823 ) ;
#3473 = FACE_OUTER_BOUND ( 'NONE', #3973, .T. ) ;
#3474 = EDGE_LOOP ( 'NONE', ( #1564, #198 ) ) ;
#3475 = EDGE_CURVE ( 'NONE', #3810, #4351, #1474, .T. ) ;
#3476 = DIRECTION ( 'NONE',  ( 0.000000000000000000, 0.000000000000000000, -1.000000000000000000 ) ) ;
#3477 = EDGE_CURVE ( 'NONE', #4758, #553, #3016, .T. ) ;
#3478 = ADVANCED_FACE ( 'NONE', ( #2258 ), #3782, .F. ) ;
#3479 = AXIS2_PLACEMENT_3D ( 'NONE', #3702, #281, #1347 ) ;
#3480 = LINE ( 'NONE', #1568, #317 ) ;
#3481 = DIRECTION ( 'NONE',  ( 0.000000000000000000, 1.000000000000000000, -1.467581828789149532E-15 ) ) ;
#3482 = ORIENTED_EDGE ( 'NONE', *, *, #2385, .T. ) ;
#3483 = ORIENTED_EDGE ( 'NONE', *, *, #2316, .T. ) ;
#3484 = ADVANCED_FACE ( 'NONE', ( #2411, #3905 ), #3559, .F. ) ;
#3485 = CARTESIAN_POINT ( 'NONE',  ( 22.76902711785762889, 10.32479573876449130, -27.98806281106213589 ) ) ;
#3486 = CARTESIAN_POINT ( 'NONE',  ( -2.172477277502393807E-14, 16.00000000000000000, -28.09999999999999787 ) ) ;
#3487 = CARTESIAN_POINT ( 'NONE',  ( 2.000000000000000000, -1.773042676681340968, 2.059984127722458425E-15 ) ) ;
#3488 = ORIENTED_EDGE ( 'NONE', *, *, #749, .F. ) ;
#3489 = ORIENTED_EDGE ( 'NONE', *, *, #939, .T. ) ;
#3490 = APPLICATION_PROTOCOL_DEFINITION ( 'draft international standard', 'automotive_design', 1998, #1025 ) ;
#3491 = DIRECTION ( 'NONE',  ( 0.000000000000000000, 0.000000000000000000, 1.000000000000000000 ) ) ;
#3492 = LINE ( 'NONE', #3943, #4004 ) ;
#3493 = CARTESIAN_POINT ( 'NONE',  ( 2.302289838212012812E-14, -16.00000000000000000, -23.90000000000001279 ) ) ;
#3494 = VERTEX_POINT ( 'NONE', #878 ) ;
#3495 = EDGE_LOOP ( 'NONE', ( #4555, #1091, #1113, #3136 ) ) ;
#3496 = LINE ( 'NONE', #1969, #4242 ) ;
#3497 = DIRECTION ( 'NONE',  ( 0.000000000000000000, -0.5000000000000011102, -0.8660254037844379305 ) ) ;
#3498 = DIRECTION ( 'NONE',  ( -1.000000000000000000, 0.000000000000000000, 0.000000000000000000 ) ) ;
#3499 = ORIENTED_EDGE ( 'NONE', *, *, #1951, .T. ) ;
#3500 = DIRECTION ( 'NONE',  ( 0.000000000000000000, 0.4999999999999993339, -0.8660254037844390407 ) ) ;
#3501 = DIRECTION ( 'NONE',  ( 0.000000000000000000, 1.000000000000000000, -1.471414886128461471E-15 ) ) ;
#3502 = ORIENTED_EDGE ( 'NONE', *, *, #4768, .T. ) ;
#3503 = ORIENTED_EDGE ( 'NONE', *, *, #3648, .T. ) ;
#3504 = CARTESIAN_POINT ( 'NONE',  ( 22.52496067886514552, -10.84608396733234237, -29.07843770730522337 ) ) ;
#3505 = ADVANCED_FACE ( 'NONE', ( #2084 ), #657, .T. ) ;
#3506 = AXIS2_PLACEMENT_3D ( 'NONE', #3412, #2235, #4947 ) ;
#3507 = CARTESIAN_POINT ( 'NONE',  ( -19.30673457630776824, 12.50000000000006750, -12.00000000000000000 ) ) ;
#3508 = EDGE_CURVE ( 'NONE', #4266, #3027, #4417, .T. ) ;
#3509 = LINE ( 'NONE', #1599, #4331 ) ;
#3510 = ORIENTED_EDGE ( 'NONE', *, *, #4141, .T. ) ;
#3511 = ORIENTED_EDGE ( 'NONE', *, *, #1360, .T. ) ;
#3512 = CARTESIAN_POINT ( 'NONE',  ( 0.000000000000000000, 0.000000000000000000, 4.000000000000000000 ) ) ;
#3513 = CARTESIAN_POINT ( 'NONE',  ( -16.10609822396473945, -5.439999999999995062, 14.30577747056276472 ) ) ;
#3514 = CARTESIAN_POINT ( 'NONE',  ( 21.90822715901080642, -12.04290832652441168, -21.39512301784776227 ) ) ;
#3515 = ORIENTED_EDGE ( 'NONE', *, *, #3411, .F. ) ;
#3516 = ORIENTED_EDGE ( 'NONE', *, *, #3318, .T. ) ;
#3517 =( LENGTH_UNIT ( ) NAMED_UNIT ( * ) SI_UNIT ( .MILLI., .METRE. ) );
#3518 = DIRECTION ( 'NONE',  ( 1.000000000000000000, -7.105427357601001859E-15, 0.000000000000000000 ) ) ;
#3519 = CARTESIAN_POINT ( 'NONE',  ( 2.500000000000000000, -1.178949249685213863, 2.042000000000002924 ) ) ;
#3520 = CARTESIAN_POINT ( 'NONE',  ( 15.00000000000000000, -16.00000000000000000, -20.00000000000000000 ) ) ;
#3521 = ORIENTED_EDGE ( 'NONE', *, *, #4025, .F. ) ;
#3522 = LINE ( 'NONE', #4352, #3044 ) ;
#3523 = CARTESIAN_POINT ( 'NONE',  ( 2.444036937190193033E-14, 6.999999999999999112, -32.00000000000000000 ) ) ;
#3524 = AXIS2_PLACEMENT_3D ( 'NONE', #395, #1921, #2277 ) ;
#3525 = EDGE_LOOP ( 'NONE', ( #2940, #3091, #827, #1957 ) ) ;
#3526 = ORIENTED_EDGE ( 'NONE', *, *, #2270, .F. ) ;
#3527 = CIRCLE ( 'NONE', #3216, 3.500000000000000000 ) ;
#3528 = EDGE_CURVE ( 'NONE', #3847, #1283, #488, .T. ) ;
#3529 = ADVANCED_FACE ( 'NONE', ( #1980 ), #909, .T. ) ;
#3530 = CARTESIAN_POINT ( 'NONE',  ( 2.000000000000000000, 1.773042676681340968, -2.276824562219559311E-15 ) ) ;
#3531 = VECTOR ( 'NONE', #1965, 1000.000000000000000 ) ;
#3532 = CARTESIAN_POINT ( 'NONE',  ( 22.18564505841182211, -11.52792329777113878, -21.98172240441969905 ) ) ;
#3533 = AXIS2_PLACEMENT_3D ( 'NONE', #3542, #3866, #1985 ) ;
#3534 = CARTESIAN_POINT ( 'NONE',  ( -14.00000000000006395, 16.00000000000000000, -23.90000000000000568 ) ) ;
#3535 = LINE ( 'NONE', #106, #12 ) ;
#3536 = VERTEX_POINT ( 'NONE', #3534 ) ;
#3537 = ORIENTED_EDGE ( 'NONE', *, *, #4639, .F. ) ;
#3538 = VECTOR ( 'NONE', #1463, 1000.000000000000000 ) ;
#3539 = CIRCLE ( 'NONE', #1373, 22.99999999999998934 ) ;
#3540 = EDGE_CURVE ( 'NONE', #3700, #165, #2814, .T. ) ;
#3541 = CONTEXT_DEPENDENT_SHAPE_REPRESENTATION ( #1798, #1124 ) ;
#3542 = CARTESIAN_POINT ( 'NONE',  ( 0.000000000000000000, 0.000000000000000000, 4.000000000000000000 ) ) ;
#3543 = LINE ( 'NONE', #3513, #809 ) ;
#3544 = CARTESIAN_POINT ( 'NONE',  ( 0.000000000000000000, 0.000000000000000000, 12.00000000000000000 ) ) ;
#3545 = ORIENTED_EDGE ( 'NONE', *, *, #4181, .F. ) ;
#3546 = EDGE_CURVE ( 'NONE', #451, #374, #2039, .T. ) ;
#3547 = AXIS2_PLACEMENT_3D ( 'NONE', #1677, #4308, #556 ) ;
#3548 = ORIENTED_EDGE ( 'NONE', *, *, #684, .T. ) ;
#3549 = DIRECTION ( 'NONE',  ( -0.000000000000000000, -0.000000000000000000, -1.000000000000000000 ) ) ;
#3550 = DIRECTION ( 'NONE',  ( 1.000000000000000000, -0.000000000000000000, -0.000000000000000000 ) ) ;
#3551 = CARTESIAN_POINT ( 'NONE',  ( 2.500000000000000000, 1.178949249685213863, -2.042000000000001148 ) ) ;
#3552 = AXIS2_PLACEMENT_3D ( 'NONE', #868, #142, #1666 ) ;
#3553 = EDGE_LOOP ( 'NONE', ( #23, #2361, #1656, #2402, #3562, #180 ) ) ;
#3554 = DIRECTION ( 'NONE',  ( -1.000000000000000000, -0.000000000000000000, -0.000000000000000000 ) ) ;
#3555 = CARTESIAN_POINT ( 'NONE',  ( 0.000000000000000000, 1.773042676681340968, -2.276824562219559311E-15 ) ) ;
#3556 = ORIENTED_EDGE ( 'NONE', *, *, #548, .T. ) ;
#3557 = CARTESIAN_POINT ( 'NONE',  ( -11.26180729995785157, -16.00000000000000355, -26.00000000000000355 ) ) ;
#3558 =( LENGTH_UNIT ( ) NAMED_UNIT ( * ) SI_UNIT ( .MILLI., .METRE. ) );
#3559 = PLANE ( 'NONE',  #2586 ) ;
#3560 = EDGE_CURVE ( 'NONE', #406, #1430, #1780, .T. ) ;
#3561 = ORIENTED_EDGE ( 'NONE', *, *, #3468, .F. ) ;
#3562 = ORIENTED_EDGE ( 'NONE', *, *, #1060, .T. ) ;
#3563 = DIRECTION ( 'NONE',  ( 0.000000000000000000, 0.000000000000000000, -1.000000000000000000 ) ) ;
#3564 = LINE ( 'NONE', #1583, #2977 ) ;
#3565 = DIRECTION ( 'NONE',  ( 1.000000000000000000, 0.000000000000000000, 0.000000000000000000 ) ) ;
#3566 = ADVANCED_FACE ( 'NONE', ( #105 ), #2510, .F. ) ;
#3567 = ORIENTED_EDGE ( 'NONE', *, *, #4669, .T. ) ;
#3568 = ORIENTED_EDGE ( 'NONE', *, *, #4039, .T. ) ;
#3569 = CARTESIAN_POINT ( 'NONE',  ( 2.000000000000000000, 0.8865213383406685965, -1.535500000000000753 ) ) ;
#3570 = FACE_OUTER_BOUND ( 'NONE', #125, .T. ) ;
#3571 = PLANE ( 'NONE',  #3552 ) ;
#3572 = EDGE_CURVE ( 'NONE', #553, #4747, #1062, .T. ) ;
#3573 = EDGE_CURVE ( 'NONE', #4351, #1209, #4333, .T. ) ;
#3574 = ORIENTED_EDGE ( 'NONE', *, *, #1361, .F. ) ;
#3575 = FACE_OUTER_BOUND ( 'NONE', #4112, .T. ) ;
#3576 = CARTESIAN_POINT ( 'NONE',  ( 2.444036937190193033E-14, 6.999999999999999112, -32.00000000000000000 ) ) ;
#3577 = ORIENTED_EDGE ( 'NONE', *, *, #2585, .T. ) ;
#3578 = LINE ( 'NONE', #149, #841 ) ;
#3579 = SURFACE_STYLE_USAGE ( .BOTH. , #4763 ) ;
#3580 = DIRECTION ( 'NONE',  ( 0.000000000000000000, 0.000000000000000000, 1.000000000000000000 ) ) ;
#3581 = ORIENTED_EDGE ( 'NONE', *, *, #1758, .F. ) ;
#3582 = ORIENTED_EDGE ( 'NONE', *, *, #2870, .F. ) ;
#3583 = ADVANCED_FACE ( 'NONE', ( #50 ), #3075, .F. ) ;
#3584 = CARTESIAN_POINT ( 'NONE',  ( 24.00000000000000000, 0.000000000000000000, 0.000000000000000000 ) ) ;
#3585 = LINE ( 'NONE', #936, #3144 ) ;
#3586 = DIRECTION ( 'NONE',  ( 1.000000000000000000, 1.106769389831504682E-16, -0.000000000000000000 ) ) ;
#3587 = EDGE_LOOP ( 'NONE', ( #3179, #4284, #3502, #2300, #1355, #782, #4387, #84, #4577 ) ) ;
#3588 = ORIENTED_EDGE ( 'NONE', *, *, #1278, .T. ) ;
#3589 = DIRECTION ( 'NONE',  ( 1.000000000000000000, -0.000000000000000000, -0.000000000000000000 ) ) ;
#3590 = CARTESIAN_POINT ( 'NONE',  ( 22.04417985544612790, 11.79351823160730461, -20.25405616187230962 ) ) ;
#3591 = CARTESIAN_POINT ( 'NONE',  ( -31.74999999999995737, 0.000000000000000000, 4.250000000000000000 ) ) ;
#3592 = ORIENTED_EDGE ( 'NONE', *, *, #1917, .F. ) ;
#3593 = VECTOR ( 'NONE', #2863, 1000.000000000000000 ) ;
#3594 = CARTESIAN_POINT ( 'NONE',  ( 0.000000000000000000, 0.000000000000000000, -4.000000000000000000 ) ) ;
#3595 = CARTESIAN_POINT ( 'NONE',  ( -14.00000000000006395, 16.00000000000000000, -26.00000000000000355 ) ) ;
#3596 = ORIENTED_EDGE ( 'NONE', *, *, #1515, .F. ) ;
#3597 = ADVANCED_FACE ( 'NONE', ( #2062 ), #4255, .F. ) ;
#3598 = TOROIDAL_SURFACE ( 'NONE', #4554, 4.000000000000000000, 0.2500000000000000000 ) ;
#3599 = EDGE_CURVE ( 'NONE', #3261, #1067, #932, .T. ) ;
#3600 = DIRECTION ( 'NONE',  ( 0.000000000000000000, 0.000000000000000000, 1.000000000000000000 ) ) ;
#3601 = AXIS2_PLACEMENT_3D ( 'NONE', #1540, #1270, #3949 ) ;
#3602 = ORIENTED_EDGE ( 'NONE', *, *, #4116, .F. ) ;
#3603 = VERTEX_POINT ( 'NONE', #2364 ) ;
#3604 = AXIS2_PLACEMENT_3D ( 'NONE', #445, #2746, #1167 ) ;
#3605 = AXIS2_PLACEMENT_3D ( 'NONE', #703, #4868, #4157 ) ;
#3606 = DIRECTION ( 'NONE',  ( 1.000000000000000000, 0.000000000000000000, 0.000000000000000000 ) ) ;
#3607 = CARTESIAN_POINT ( 'NONE',  ( 8.500000000000001776, -9.407539813567788568E-16, 12.00000000000000000 ) ) ;
#3608 = DIRECTION ( 'NONE',  ( -0.9474175425861605104, -0.3200000000000010059, 0.000000000000000000 ) ) ;
#3609 = MANIFOLD_SOLID_BREP ( 'M5 Tapped Hole1', #3163 ) ;
#3610 = AXIS2_PLACEMENT_3D ( 'NONE', #3942, #3606, #1709 ) ;
#3611 = VERTEX_POINT ( 'NONE', #179 ) ;
#3612 = ORIENTED_EDGE ( 'NONE', *, *, #2585, .F. ) ;
#3613 = AXIS2_PLACEMENT_3D ( 'NONE', #4514, #4140, #710 ) ;
#3614 = VECTOR ( 'NONE', #29, 1000.000000000000000 ) ;
#3615 = DIRECTION ( 'NONE',  ( 0.000000000000000000, 0.000000000000000000, -1.000000000000000000 ) ) ;
#3616 = DIRECTION ( 'NONE',  ( 1.000000000000000000, -0.000000000000000000, -0.000000000000000000 ) ) ;
#3617 = DIRECTION ( 'NONE',  ( 0.000000000000000000, 0.000000000000000000, -1.000000000000000000 ) ) ;
#3618 = ORIENTED_EDGE ( 'NONE', *, *, #3175, .T. ) ;
#3619 = CIRCLE ( 'NONE', #1457, 25.00000000000000000 ) ;
#3620 = CARTESIAN_POINT ( 'NONE',  ( 25.00000000000000000, 0.000000000000000000, 0.000000000000000000 ) ) ;
#3621 = DIRECTION ( 'NONE',  ( 1.000000000000000000, 0.000000000000000000, 0.000000000000000000 ) ) ;
#3622 = LINE ( 'NONE', #4566, #3284 ) ;
#3623 = AXIS2_PLACEMENT_3D ( 'NONE', #3662, #1483, #3342 ) ;
#3624 = EDGE_LOOP ( 'NONE', ( #3838, #1972 ) ) ;
#3625 = ADVANCED_FACE ( 'NONE', ( #3672, #3884 ), #4807, .T. ) ;
#3626 = DIRECTION ( 'NONE',  ( 0.000000000000000000, 0.000000000000000000, -1.000000000000000000 ) ) ;
#3627 = DIRECTION ( 'NONE',  ( 0.000000000000000000, 0.000000000000000000, 1.000000000000000000 ) ) ;
#3628 = CARTESIAN_POINT ( 'NONE',  ( 15.00000000000000000, 11.80087472665740300, -30.28571428571428470 ) ) ;
#3629 = EDGE_CURVE ( 'NONE', #1649, #3812, #2346, .T. ) ;
#3630 = ORIENTED_EDGE ( 'NONE', *, *, #802, .F. ) ;
#3631 = AXIS2_PLACEMENT_3D ( 'NONE', #2157, #3310, #2511 ) ;
#3632 = PLANE ( 'NONE',  #4168 ) ;
#3633 = DIRECTION ( 'NONE',  ( -1.000000000000000000, 0.000000000000000000, 0.000000000000000000 ) ) ;
#3634 = CARTESIAN_POINT ( 'NONE',  ( -13.99999999999993250, -16.00000000000000000, -28.10000000000000142 ) ) ;
#3635 = ORIENTED_EDGE ( 'NONE', *, *, #3175, .F. ) ;
#3636 = ORIENTED_EDGE ( 'NONE', *, *, #2140, .T. ) ;
#3637 =( NAMED_UNIT ( * ) SI_UNIT ( $, .STERADIAN. ) SOLID_ANGLE_UNIT ( ) );
#3638 = CARTESIAN_POINT ( 'NONE',  ( -23.00000000000000711, 0.000000000000000000, 4.000000000000000000 ) ) ;
#3639 = LINE ( 'NONE', #3320, #4648 ) ;
#3640 = VERTEX_POINT ( 'NONE', #3703 ) ;
#3641 = DIRECTION ( 'NONE',  ( -0.000000000000000000, -0.000000000000000000, 1.000000000000000000 ) ) ;
#3642 = ORIENTED_EDGE ( 'NONE', *, *, #4142, .F. ) ;
#3643 = LINE ( 'NONE', #1364, #2086 ) ;
#3644 = CARTESIAN_POINT ( 'NONE',  ( 23.61000000000001364, 0.000000000000000000, 0.000000000000000000 ) ) ;
#3645 = ORIENTED_EDGE ( 'NONE', *, *, #99, .F. ) ;
#3646 = LINE ( 'NONE', #4027, #1715 ) ;
#3647 = PRODUCT_CONTEXT ( 'NONE', #3945, 'mechanical' ) ;
#3648 = EDGE_CURVE ( 'NONE', #4131, #4716, #1803, .T. ) ;
#3649 = LINE ( 'NONE', #514, #4571 ) ;
#3650 = CARTESIAN_POINT ( 'NONE',  ( -3.642919299551294898E-14, 16.00000000000000000, -26.00000000000000355 ) ) ;
#3651 = EDGE_LOOP ( 'NONE', ( #919, #4633, #2752 ) ) ;
#3652 = ADVANCED_FACE ( 'NONE', ( #1566 ), #321, .F. ) ;
#3653 = EDGE_CURVE ( 'NONE', #4296, #1395, #3130, .T. ) ;
#3654 = EDGE_CURVE ( 'NONE', #2615, #1050, #3381, .T. ) ;
#3655 = CARTESIAN_POINT ( 'NONE',  ( -9.000000000000001776, 2.000000000000000000, -32.00000000000000000 ) ) ;
#3656 = CYLINDRICAL_SURFACE ( 'NONE', #101, 25.00000000000000000 ) ;
#3657 = VERTEX_POINT ( 'NONE', #2376 ) ;
#3658 = ADVANCED_FACE ( 'NONE', ( #3844 ), #1173, .T. ) ;
#3659 = VERTEX_POINT ( 'NONE', #4241 ) ;
#3660 = LINE ( 'NONE', #4413, #4326 ) ;
#3661 = CARTESIAN_POINT ( 'NONE',  ( 21.86452818504794138, 12.12206676558875529, -20.99167230228674441 ) ) ;
#3662 = CARTESIAN_POINT ( 'NONE',  ( 0.000000000000000000, 0.000000000000000000, -12.00000000000000000 ) ) ;
#3663 = ORIENTED_EDGE ( 'NONE', *, *, #2216, .F. ) ;
#3664 = CARTESIAN_POINT ( 'NONE',  ( -13.99999999999993250, -16.00000000000000000, -23.90000000000000568 ) ) ;
#3665 = DIRECTION ( 'NONE',  ( -1.000000000000000000, -0.000000000000000000, -0.000000000000000000 ) ) ;
#3666 = CIRCLE ( 'NONE', #957, 25.00000000000000000 ) ;
#3667 = ORIENTED_EDGE ( 'NONE', *, *, #1645, .T. ) ;
#3668 = DIRECTION ( 'NONE',  ( -0.000000000000000000, -1.000000000000000000, -0.000000000000000000 ) ) ;
#3669 = CIRCLE ( 'NONE', #2559, 2.500000000000001332 ) ;
#3670 = DIRECTION ( 'NONE',  ( 1.000000000000000000, 0.000000000000000000, 0.000000000000000000 ) ) ;
#3671 = LINE ( 'NONE', #223, #3699 ) ;
#3672 = FACE_BOUND ( 'NONE', #356, .T. ) ;
#3673 = ORIENTED_EDGE ( 'NONE', *, *, #2930, .T. ) ;
#3674 = AXIS2_PLACEMENT_3D ( 'NONE', #595, #3665, #615 ) ;
#3675 = EDGE_CURVE ( 'NONE', #3891, #2240, #2912, .T. ) ;
#3676 =( REPRESENTATION_RELATIONSHIP ('NONE','NONE', #137, #4748 ) REPRESENTATION_RELATIONSHIP_WITH_TRANSFORMATION ( #3012 )SHAPE_REPRESENTATION_RELATIONSHIP( ) );
#3677 = CARTESIAN_POINT ( 'NONE',  ( 23.68543856465402797, 7.999999999999996447, -4.000000000000000000 ) ) ;
#3678 = AXIS2_PLACEMENT_3D ( 'NONE', #2723, #2023, #475 ) ;
#3679 = CARTESIAN_POINT ( 'NONE',  ( 0.000000000000000000, -25.00000000000000000, -32.00000000000000000 ) ) ;
#3680 = CARTESIAN_POINT ( 'NONE',  ( 2.000000000000000000, -0.8865213383406690406, 1.535500000000000975 ) ) ;
#3681 = ADVANCED_FACE ( 'NONE', ( #1440 ), #1845, .T. ) ;
#3682 = EDGE_CURVE ( 'NONE', #2782, #2020, #3619, .T. ) ;
#3683 = ORIENTED_EDGE ( 'NONE', *, *, #3119, .F. ) ;
#3684 = AXIS2_PLACEMENT_3D ( 'NONE', #214, #1734, #4795 ) ;
#3685 = TOROIDAL_SURFACE ( 'NONE', #3767, 3.299999999999999822, 0.2000000000000000111 ) ;
#3686 = CARTESIAN_POINT ( 'NONE',  ( 6.999999999999999112, 0.000000000000000000, -12.00000000000000000 ) ) ;
#3687 = DIRECTION ( 'NONE',  ( 0.000000000000000000, 0.000000000000000000, 1.000000000000000000 ) ) ;
#3688 = FACE_OUTER_BOUND ( 'NONE', #2008, .T. ) ;
#3689 = VECTOR ( 'NONE', #27, 1000.000000000000000 ) ;
#3690 = CARTESIAN_POINT ( 'NONE',  ( 2.444036937190193033E-14, 6.999999999999999112, -32.00000000000000000 ) ) ;
#3691 = VECTOR ( 'NONE', #1423, 1000.000000000000114 ) ;
#3692 = VERTEX_POINT ( 'NONE', #846 ) ;
#3693 = AXIS2_PLACEMENT_3D ( 'NONE', #2174, #1040, #4538 ) ;
#3694 = AXIS2_PLACEMENT_3D ( 'NONE', #3544, #2488, #3565 ) ;
#3695 = VECTOR ( 'NONE', #132, 1000.000000000000000 ) ;
#3696 = LINE ( 'NONE', #1506, #3538 ) ;
#3697 = DIRECTION ( 'NONE',  ( -0.000000000000000000, -0.000000000000000000, 1.000000000000000000 ) ) ;
#3698 = DIRECTION ( 'NONE',  ( 0.000000000000000000, 0.000000000000000000, -1.000000000000000000 ) ) ;
#3699 = VECTOR ( 'NONE', #4212, 1000.000000000000000 ) ;
#3700 = VERTEX_POINT ( 'NONE', #4497 ) ;
#3701 = AXIS2_PLACEMENT_3D ( 'NONE', #4349, #1389, #4870 ) ;
#3702 = CARTESIAN_POINT ( 'NONE',  ( 0.000000000000000000, 0.000000000000000000, -32.00000000000000000 ) ) ;
#3703 = CARTESIAN_POINT ( 'NONE',  ( 25.00000000000000000, 0.000000000000000000, -20.00000000000000000 ) ) ;
#3704 = VERTEX_POINT ( 'NONE', #423 ) ;
#3705 = EDGE_CURVE ( 'NONE', #2615, #1989, #477, .T. ) ;
#3706 = CARTESIAN_POINT ( 'NONE',  ( 2.000000000000000000, -1.773042676681340968, 2.059984127722458425E-15 ) ) ;
#3707 = CARTESIAN_POINT ( 'NONE',  ( 15.00000000000000000, 16.00000000000000000, -23.35000000000000853 ) ) ;
#3708 = DIRECTION ( 'NONE',  ( -1.000000000000000000, 0.000000000000000000, -0.000000000000000000 ) ) ;
#3709 = EDGE_LOOP ( 'NONE', ( #2925, #969, #1775, #3667 ) ) ;
#3710 = CIRCLE ( 'NONE', #1553, 1.535500000000000087 ) ;
#3711 = CARTESIAN_POINT ( 'NONE',  ( 2.000000000000000000, 1.773042676681340968, -2.276824562219559311E-15 ) ) ;
#3712 = SURFACE_SIDE_STYLE ('',( #681 ) ) ;
#3713 = EDGE_CURVE ( 'NONE', #3603, #2165, #1224, .T. ) ;
#3714 = DIRECTION ( 'NONE',  ( -0.000000000000000000, -0.000000000000000000, -1.000000000000000000 ) ) ;
#3715 = PRODUCT_RELATED_PRODUCT_CATEGORY ( 'part', '', ( #853 ) ) ;
#3716 = CARTESIAN_POINT ( 'NONE',  ( -14.00000000000006395, 16.00000000000000000, -26.00000000000000355 ) ) ;
#3717 = EDGE_CURVE ( 'NONE', #4613, #1731, #4258, .T. ) ;
#3718 = ORIENTED_EDGE ( 'NONE', *, *, #3572, .F. ) ;
#3719 = DIRECTION ( 'NONE',  ( 0.000000000000000000, 0.000000000000000000, 1.000000000000000000 ) ) ;
#3720 = SHAPE_REPRESENTATION ( 'Output Clamping Hub Sleeve', ( #1918 ), #4450 ) ;
#3721 = EDGE_LOOP ( 'NONE', ( #3465, #4334, #2642, #977, #3307, #4257 ) ) ;
#3722 = DIRECTION ( 'NONE',  ( 0.000000000000000000, 0.000000000000000000, -1.000000000000000000 ) ) ;
#3723 = LINE ( 'NONE', #593, #3998 ) ;
#3724 = CARTESIAN_POINT ( 'NONE',  ( 0.000000000000000000, 0.000000000000000000, -32.00000000000000000 ) ) ;
#3725 = EDGE_CURVE ( 'NONE', #1262, #374, #1625, .T. ) ;
#3726 = DIRECTION ( 'NONE',  ( -1.000000000000000000, 0.000000000000000000, 0.000000000000000000 ) ) ;
#3727 = DIRECTION ( 'NONE',  ( 0.000000000000000000, 0.5000000000000012212, 0.8660254037844380415 ) ) ;
#3728 = CYLINDRICAL_SURFACE ( 'NONE', #4345, 22.99999999999998934 ) ;
#3729 = ORIENTED_EDGE ( 'NONE', *, *, #4261, .T. ) ;
#3730 = PLANE ( 'NONE',  #2744 ) ;
#3731 = PLANE ( 'NONE',  #727 ) ;
#3732 = EDGE_LOOP ( 'NONE', ( #4139, #1898, #2263, #3344 ) ) ;
#3733 = ORIENTED_EDGE ( 'NONE', *, *, #1182, .T. ) ;
#3734 = DIRECTION ( 'NONE',  ( -1.000000000000000000, -0.000000000000000000, -0.000000000000000000 ) ) ;
#3735 = LINE ( 'NONE', #3341, #2820 ) ;
#3736 = DIRECTION ( 'NONE',  ( -0.000000000000000000, -0.000000000000000000, 1.000000000000000000 ) ) ;
#3737 = COLOUR_RGB ( '', 0.08235294, 0.09019608, 0.10196078) ;
#3738 = ORIENTED_EDGE ( 'NONE', *, *, #4025, .T. ) ;
#3739 = CARTESIAN_POINT ( 'NONE',  ( 12.50000000000000178, 19.30673457630782863, 4.000000000000000000 ) ) ;
#3740 = CARTESIAN_POINT ( 'NONE',  ( 2.500000000000000000, 0.000000000000000000, 0.000000000000000000 ) ) ;
#3741 = ORIENTED_EDGE ( 'NONE', *, *, #1240, .T. ) ;
#3742 = EDGE_CURVE ( 'NONE', #4175, #2273, #518, .T. ) ;
#3743 = DIRECTION ( 'NONE',  ( -1.000000000000000000, -3.784637517658031179E-16, -0.000000000000000000 ) ) ;
#3744 = DIRECTION ( 'NONE',  ( 1.000000000000000000, 2.168404344971009361E-16, 0.000000000000000000 ) ) ;
#3745 = ITEM_DEFINED_TRANSFORMATION ( 'NONE', 'NONE', #2394,  #1918 ) ;
#3746 = DIRECTION ( 'NONE',  ( 0.000000000000000000, 0.000000000000000000, -1.000000000000000000 ) ) ;
#3747 = VERTEX_POINT ( 'NONE', #3013 ) ;
#3748 = EDGE_CURVE ( 'NONE', #297, #4198, #1251, .T. ) ;
#3749 = AXIS2_PLACEMENT_3D ( 'NONE', #3924, #2454, #3234 ) ;
#3750 = DIRECTION ( 'NONE',  ( 0.000000000000000000, 0.000000000000000000, -1.000000000000000000 ) ) ;
#3751 = CARTESIAN_POINT ( 'NONE',  ( -9.000000000000001776, 2.000000000000000000, -32.00000000000000000 ) ) ;
#3752 = DIRECTION ( 'NONE',  ( 0.000000000000000000, -0.8660254037844390407, -0.4999999999999993339 ) ) ;
#3753 = CARTESIAN_POINT ( 'NONE',  ( 23.68543856465402442, -8.000000000000003553, 14.30577747056276472 ) ) ;
#3754 = VERTEX_POINT ( 'NONE', #1619 ) ;
#3755 = PRODUCT_DEFINITION_SHAPE ( 'NONE', 'NONE',  #4968 ) ;
#3756 = AXIS2_PLACEMENT_3D ( 'NONE', #147, #825, #1200 ) ;
#3757 = ORIENTED_EDGE ( 'NONE', *, *, #1366, .F. ) ;
#3758 = DIRECTION ( 'NONE',  ( 9.765537692533071851E-17, -9.974667427877440261E-17, 1.000000000000000000 ) ) ;
#3759 = DIRECTION ( 'NONE',  ( 1.000000000000000000, -0.000000000000000000, -0.000000000000000000 ) ) ;
#3760 = DIRECTION ( 'NONE',  ( 1.000000000000000000, 0.000000000000000000, 0.000000000000000000 ) ) ;
#3761 = CARTESIAN_POINT ( 'NONE',  ( 23.61000000000001364, 2.449293598294707400E-16, -2.000000000000000444 ) ) ;
#3762 = AXIS2_PLACEMENT_3D ( 'NONE', #3842, #2778, #4211 ) ;
#3763 = ORIENTED_EDGE ( 'NONE', *, *, #3528, .T. ) ;
#3764 = DIRECTION ( 'NONE',  ( -1.000000000000000000, -0.000000000000000000, -0.000000000000000000 ) ) ;
#3765 = AXIS2_PLACEMENT_3D ( 'NONE', #2266, #2194, #1502 ) ;
#3766 = CARTESIAN_POINT ( 'NONE',  ( 15.00000000000000000, 11.10102051443364424, -20.00000000000000000 ) ) ;
#3767 = AXIS2_PLACEMENT_3D ( 'NONE', #1137, #4185, #3687 ) ;
#3768 = ADVANCED_FACE ( 'NONE', ( #4213 ), #788, .F. ) ;
#3769 = ORIENTED_EDGE ( 'NONE', *, *, #113, .F. ) ;
#3770 = AXIS2_PLACEMENT_3D ( 'NONE', #1208, #2769, #798 ) ;
#3771 = AXIS2_PLACEMENT_3D ( 'NONE', #2888, #4032, #581 ) ;
#3772 = DIRECTION ( 'NONE',  ( 0.000000000000000000, 0.000000000000000000, -1.000000000000000000 ) ) ;
#3773 = CARTESIAN_POINT ( 'NONE',  ( 2.000000000000000000, -1.329782007511004727, 0.7677500000000014868 ) ) ;
#3774 = AXIS2_PLACEMENT_3D ( 'NONE', #2269, #4096, #1816 ) ;
#3775 = VECTOR ( 'NONE', #1729, 1000.000000000000000 ) ;
#3776 = STYLED_ITEM ( 'NONE', ( #620 ), #2079 ) ;
#3777 = EDGE_CURVE ( 'NONE', #1968, #1919, #41, .T. ) ;
#3778 = ORIENTED_EDGE ( 'NONE', *, *, #1576, .F. ) ;
#3779 = AXIS2_PLACEMENT_3D ( 'NONE', #2688, #772, #3093 ) ;
#3780 = DIRECTION ( 'NONE',  ( -1.000000000000000000, -1.357798298438996130E-15, 0.000000000000000000 ) ) ;
#3781 = ADVANCED_FACE ( 'NONE', ( #3473 ), #3728, .T. ) ;
#3782 = CYLINDRICAL_SURFACE ( 'NONE', #2435, 17.00000000000000000 ) ;
#3783 = DIRECTION ( 'NONE',  ( -1.106769389831504313E-16, -1.000000000000000000, 0.000000000000000000 ) ) ;
#3784 = CONICAL_SURFACE ( 'NONE', #2589, 1.610000000000000098, 0.7853981633974647103 ) ;
#3785 = CARTESIAN_POINT ( 'NONE',  ( -6.708203932499366751, -2.000000000000003553, -20.00000000000000000 ) ) ;
#3786 = ORIENTED_EDGE ( 'NONE', *, *, #4533, .F. ) ;
#3787 = CARTESIAN_POINT ( 'NONE',  ( -13.99999999999993250, -16.00000000000000000, -28.10000000000000142 ) ) ;
#3788 = DIRECTION ( 'NONE',  ( 1.000000000000000000, 0.000000000000000000, 0.000000000000000000 ) ) ;
#3789 = CARTESIAN_POINT ( 'NONE',  ( 2.000000000000000000, 1.880445160090761061E-16, -1.535500000000000087 ) ) ;
#3790 = ORIENTED_EDGE ( 'NONE', *, *, #930, .T. ) ;
#3791 = DIRECTION ( 'NONE',  ( -1.000000000000000000, -0.000000000000000000, -0.000000000000000000 ) ) ;
#3792 = VECTOR ( 'NONE', #2550, 1000.000000000000114 ) ;
#3793 = CARTESIAN_POINT ( 'NONE',  ( 0.000000000000000000, 0.000000000000000000, 4.000000000000000000 ) ) ;
#3794 = CARTESIAN_POINT ( 'NONE',  ( 2.500000000000000000, -2.357898499370432610, 3.252606517456513302E-15 ) ) ;
#3795 = ORIENTED_EDGE ( 'NONE', *, *, #4523, .T. ) ;
#3796 = CARTESIAN_POINT ( 'NONE',  ( 0.000000000000000000, 0.000000000000000000, -4.000000000000000000 ) ) ;
#3797 = CARTESIAN_POINT ( 'NONE',  ( -7.332110811570578784E-14, -6.999999999999999112, -32.00000000000000000 ) ) ;
#3798 = ORIENTED_EDGE ( 'NONE', *, *, #2952, .T. ) ;
#3799 = CARTESIAN_POINT ( 'NONE',  ( 23.68543856465402797, 7.999999999999996447, 14.30577747056276472 ) ) ;
#3800 = DIRECTION ( 'NONE',  ( 0.000000000000000000, 0.000000000000000000, -1.000000000000000000 ) ) ;
#3801 = DIRECTION ( 'NONE',  ( 1.000000000000000000, -0.000000000000000000, -0.000000000000000000 ) ) ;
#3802 = DIRECTION ( 'NONE',  ( 0.000000000000000000, 0.000000000000000000, -1.000000000000000000 ) ) ;
#3803 = ORIENTED_EDGE ( 'NONE', *, *, #4228, .F. ) ;
#3804 = EDGE_CURVE ( 'NONE', #1209, #3315, #2841, .T. ) ;
#3805 = CARTESIAN_POINT ( 'NONE',  ( 2.500000000000000000, 1.178949249685218525, 2.041999999999999371 ) ) ;
#3806 = SURFACE_STYLE_USAGE ( .BOTH. , #2617 ) ;
#3807 = DIRECTION ( 'NONE',  ( -1.000000000000000000, 0.000000000000000000, 0.000000000000000000 ) ) ;
#3808 = FACE_OUTER_BOUND ( 'NONE', #3651, .T. ) ;
#3809 = CARTESIAN_POINT ( 'NONE',  ( 22.04753367391287000, 11.78607713658132639, -31.73496350056613480 ) ) ;
#3810 = VERTEX_POINT ( 'NONE', #2026 ) ;
#3811 = ADVANCED_FACE ( 'NONE', ( #2879 ), #3784, .T. ) ;
#3812 = VERTEX_POINT ( 'NONE', #3201 ) ;
#3813 =( NAMED_UNIT ( * ) SI_UNIT ( $, .STERADIAN. ) SOLID_ANGLE_UNIT ( ) );
#3814 = DIRECTION ( 'NONE',  ( -0.000000000000000000, -0.000000000000000000, -1.000000000000000000 ) ) ;
#3815 = CYLINDRICAL_SURFACE ( 'NONE', #739, 3.500000000000000000 ) ;
#3816 =( GEOMETRIC_REPRESENTATION_CONTEXT ( 3 ) GLOBAL_UNCERTAINTY_ASSIGNED_CONTEXT ( ( #830 ) ) GLOBAL_UNIT_ASSIGNED_CONTEXT ( ( #3517, #4867, #4085 ) ) REPRESENTATION_CONTEXT ( 'NONE', 'WORKASPACE' ) );
#3817 = ORIENTED_EDGE ( 'NONE', *, *, #3019, .T. ) ;
#3818 = DIRECTION ( 'NONE',  ( 0.000000000000000000, 0.000000000000000000, 1.000000000000000000 ) ) ;
#3819 = DIRECTION ( 'NONE',  ( 1.000000000000000000, 0.000000000000000000, 0.000000000000000000 ) ) ;
#3820 = EDGE_LOOP ( 'NONE', ( #4368, #2939, #512, #1036 ) ) ;
#3821 = ORIENTED_EDGE ( 'NONE', *, *, #4860, .F. ) ;
#3822 = PRODUCT_DEFINITION_FORMATION_WITH_SPECIFIED_SOURCE ( 'ANY', '', #51, .NOT_KNOWN. ) ;
#3823 = CARTESIAN_POINT ( 'NONE',  ( 22.90825000241675014, 10.01062433489520132, -25.58902254984691638 ) ) ;
#3824 = LINE ( 'NONE', #3486, #4020 ) ;
#3825 = CARTESIAN_POINT ( 'NONE',  ( 2.500000000000000000, 2.357898499370433054, -1.951563910473907981E-15 ) ) ;
#3826 = CARTESIAN_POINT ( 'NONE',  ( 2.500000000000000000, 0.000000000000000000, 2.041999999999999815 ) ) ;
#3827 = EDGE_CURVE ( 'NONE', #4850, #1923, #1296, .T. ) ;
#3828 = EDGE_CURVE ( 'NONE', #597, #4842, #109, .T. ) ;
#3829 = AXIS2_PLACEMENT_3D ( 'NONE', #4275, #1920, #2706 ) ;
#3830 = EDGE_LOOP ( 'NONE', ( #4528, #858, #3237, #192 ) ) ;
#3831 = DIRECTION ( 'NONE',  ( 0.000000000000000000, -1.000000000000000000, 1.287488025362403787E-15 ) ) ;
#3832 = CIRCLE ( 'NONE', #2808, 2.000000000000000888 ) ;
#3833 = CYLINDRICAL_SURFACE ( 'NONE', #2100, 6.999999999999999112 ) ;
#3834 = CARTESIAN_POINT ( 'NONE',  ( 0.1999999999999987899, 0.000000000000000000, 3.299999999999999822 ) ) ;
#3835 = CARTESIAN_POINT ( 'NONE',  ( 22.08746549892786604, 11.71119031839157820, -31.79783224586644508 ) ) ;
#3836 = PRODUCT_RELATED_PRODUCT_CATEGORY ( 'part', '', ( #613 ) ) ;
#3837 = EDGE_CURVE ( 'NONE', #4443, #1262, #3230, .T. ) ;
#3838 = ORIENTED_EDGE ( 'NONE', *, *, #1544, .F. ) ;
#3839 = VECTOR ( 'NONE', #3851, 1000.000000000000000 ) ;
#3840 =( REPRESENTATION_RELATIONSHIP ('NONE','NONE', #137, #4221 ) REPRESENTATION_RELATIONSHIP_WITH_TRANSFORMATION ( #2607 )SHAPE_REPRESENTATION_RELATIONSHIP( ) );
#3841 = ORIENTED_EDGE ( 'NONE', *, *, #3110, .T. ) ;
#3842 = CARTESIAN_POINT ( 'NONE',  ( 0.000000000000000000, 0.000000000000000000, -4.000000000000000000 ) ) ;
#3843 = DIRECTION ( 'NONE',  ( 1.000000000000000000, 0.000000000000000000, 0.000000000000000000 ) ) ;
#3844 = FACE_OUTER_BOUND ( 'NONE', #584, .T. ) ;
#3845 = EDGE_CURVE ( 'NONE', #1283, #4766, #24, .T. ) ;
#3846 = AXIS2_PLACEMENT_3D ( 'NONE', #3793, #3814, #4143 ) ;
#3847 = VERTEX_POINT ( 'NONE', #4753 ) ;
#3848 = VECTOR ( 'NONE', #2470, 1000.000000000000000 ) ;
#3849 = AXIS2_PLACEMENT_3D ( 'NONE', #1530, #444, #2773 ) ;
#3850 = DIRECTION ( 'NONE',  ( 0.000000000000000000, 0.000000000000000000, 1.000000000000000000 ) ) ;
#3851 = DIRECTION ( 'NONE',  ( 4.073394895316987600E-15, -1.000000000000000000, 0.000000000000000000 ) ) ;
#3852 = VERTEX_POINT ( 'NONE', #3551 ) ;
#3853 = VECTOR ( 'NONE', #3038, 1000.000000000000114 ) ;
#3854 = ORIENTED_EDGE ( 'NONE', *, *, #535, .T. ) ;
#3855 = VECTOR ( 'NONE', #4783, 1000.000000000000000 ) ;
#3856 = VECTOR ( 'NONE', #4365, 1000.000000000000000 ) ;
#3857 = AXIS2_PLACEMENT_3D ( 'NONE', #951, #2512, #2410 ) ;
#3858 = CARTESIAN_POINT ( 'NONE',  ( 22.87713223651540417, 10.08160808888849047, -27.00698909695861261 ) ) ;
#3859 = DIRECTION ( 'NONE',  ( -0.7071067811865306973, 8.659560562355138702E-17, -0.7071067811865643371 ) ) ;
#3860 = FACE_OUTER_BOUND ( 'NONE', #1804, .T. ) ;
#3861 = CYLINDRICAL_SURFACE ( 'NONE', #1776, 2.500000000000000888 ) ;
#3862 = ORIENTED_EDGE ( 'NONE', *, *, #3477, .F. ) ;
#3863 = ORIENTED_EDGE ( 'NONE', *, *, #3925, .F. ) ;
#3864 = EDGE_CURVE ( 'NONE', #3812, #1649, #3236, .T. ) ;
#3865 = CARTESIAN_POINT ( 'NONE',  ( 0.000000000000000000, 0.000000000000000000, 0.000000000000000000 ) ) ;
#3866 = DIRECTION ( 'NONE',  ( 0.000000000000000000, 0.000000000000000000, 1.000000000000000000 ) ) ;
#3867 = CARTESIAN_POINT ( 'NONE',  ( 21.37171027316246708, -8.500000000000078160, -4.000000000000000000 ) ) ;
#3868 = CARTESIAN_POINT ( 'NONE',  ( 0.000000000000000000, 25.00000000000000000, -32.00000000000000000 ) ) ;
#3869 = ORIENTED_EDGE ( 'NONE', *, *, #1385, .T. ) ;
#3870 = EDGE_LOOP ( 'NONE', ( #1072, #1712, #2133, #4289 ) ) ;
#3871 = SURFACE_STYLE_USAGE ( .BOTH. , #2348 ) ;
#3872 = EDGE_CURVE ( 'NONE', #4758, #4311, #2916, .T. ) ;
#3873 = CARTESIAN_POINT ( 'NONE',  ( 0.000000000000000000, 2.357898499370433054, -1.951563910473907981E-15 ) ) ;
#3874 = FACE_OUTER_BOUND ( 'NONE', #1258, .T. ) ;
#3875 = DIRECTION ( 'NONE',  ( 0.000000000000000000, 0.000000000000000000, 1.000000000000000000 ) ) ;
#3876 = EDGE_LOOP ( 'NONE', ( #3999, #3328, #2869 ) ) ;
#3877 = AXIS2_PLACEMENT_3D ( 'NONE', #4104, #1770, #1720 ) ;
#3878 = ADVANCED_FACE ( 'NONE', ( #1735 ), #3921, .F. ) ;
#3879 = ADVANCED_FACE ( 'NONE', ( #3951, #529 ), #3571, .T. ) ;
#3880 = LINE ( 'NONE', #791, #2479 ) ;
#3881 = DIRECTION ( 'NONE',  ( 1.000000000000000000, 0.000000000000000000, 0.000000000000000000 ) ) ;
#3882 = ORIENTED_EDGE ( 'NONE', *, *, #3828, .T. ) ;
#3883 = ORIENTED_EDGE ( 'NONE', *, *, #776, .T. ) ;
#3884 = FACE_OUTER_BOUND ( 'NONE', #4809, .T. ) ;
#3885 = DIRECTION ( 'NONE',  ( -0.000000000000000000, -0.000000000000000000, -1.000000000000000000 ) ) ;
#3886 = ORIENTED_EDGE ( 'NONE', *, *, #1645, .F. ) ;
#3887 = ORIENTED_EDGE ( 'NONE', *, *, #3451, .T. ) ;
#3888 = CARTESIAN_POINT ( 'NONE',  ( 0.000000000000000000, 0.000000000000000000, -4.000000000000000000 ) ) ;
#3889 = FACE_OUTER_BOUND ( 'NONE', #4036, .T. ) ;
#3890 = DIRECTION ( 'NONE',  ( -1.000000000000000000, -1.357798298438996130E-15, 0.000000000000000000 ) ) ;
#3891 = VERTEX_POINT ( 'NONE', #4721 ) ;
#3892 = ORIENTED_EDGE ( 'NONE', *, *, #3508, .F. ) ;
#3893 =( NAMED_UNIT ( * ) SI_UNIT ( $, .STERADIAN. ) SOLID_ANGLE_UNIT ( ) );
#3894 = DIRECTION ( 'NONE',  ( 0.000000000000000000, 0.000000000000000000, 1.000000000000000000 ) ) ;
#3895 = CARTESIAN_POINT ( 'NONE',  ( 15.00000000000000000, 16.00000000000000000, -26.00000000000000355 ) ) ;
#3896 = DIRECTION ( 'NONE',  ( 0.000000000000000000, 1.000000000000000000, -1.471414886128461471E-15 ) ) ;
#3897 = EDGE_CURVE ( 'NONE', #2834, #479, #3080, .T. ) ;
#3898 = ORIENTED_EDGE ( 'NONE', *, *, #3416, .T. ) ;
#3899 = CARTESIAN_POINT ( 'NONE',  ( 0.000000000000000000, 0.000000000000000000, -32.00000000000000000 ) ) ;
#3900 = CARTESIAN_POINT ( 'NONE',  ( 0.000000000000000000, 2.357898499370433054, -1.951563910473907981E-15 ) ) ;
#3901 = EDGE_LOOP ( 'NONE', ( #3195, #1899, #1988, #3041 ) ) ;
#3902 = EDGE_CURVE ( 'NONE', #3261, #1889, #3002, .T. ) ;
#3903 = VERTEX_POINT ( 'NONE', #3322 ) ;
#3904 = CARTESIAN_POINT ( 'NONE',  ( 22.52717933085840585, 10.84147272832753828, -29.07071185665252600 ) ) ;
#3905 = FACE_OUTER_BOUND ( 'NONE', #1083, .T. ) ;
#3906 = FACE_BOUND ( 'NONE', #3624, .T. ) ;
#3907 = EDGE_CURVE ( 'NONE', #1594, #2345, #1863, .T. ) ;
#3908 = ORIENTED_EDGE ( 'NONE', *, *, #2983, .T. ) ;
#3909 = ORIENTED_EDGE ( 'NONE', *, *, #4051, .T. ) ;
#3910 = AXIS2_PLACEMENT_3D ( 'NONE', #3865, #3627, #4806 ) ;
#3911 = SHAPE_DEFINITION_REPRESENTATION ( #1774, #3720 ) ;
#3912 = FACE_OUTER_BOUND ( 'NONE', #3525, .T. ) ;
#3913 = CYLINDRICAL_SURFACE ( 'NONE', #413, 25.00000000000000000 ) ;
#3914 = CARTESIAN_POINT ( 'NONE',  ( -9.000000000000003553, -1.999999999999999112, -32.00000000000000000 ) ) ;
#3915 = VERTEX_POINT ( 'NONE', #1088 ) ;
#3916 = AXIS2_PLACEMENT_3D ( 'NONE', #1973, #372, #3425 ) ;
#3917 = EDGE_LOOP ( 'NONE', ( #4154, #2191 ) ) ;
#3918 = PRESENTATION_STYLE_ASSIGNMENT (( #3157 ) ) ;
#3919 = DIRECTION ( 'NONE',  ( 0.000000000000000000, 0.000000000000000000, 1.000000000000000000 ) ) ;
#3920 = CARTESIAN_POINT ( 'NONE',  ( 0.000000000000000000, 25.00000000000000000, -32.00000000000000000 ) ) ;
#3921 = PLANE ( 'NONE',  #279 ) ;
#3922 = CIRCLE ( 'NONE', #1752, 6.999999999999999112 ) ;
#3923 = ORIENTED_EDGE ( 'NONE', *, *, #4141, .F. ) ;
#3924 = CARTESIAN_POINT ( 'NONE',  ( 25.00000000000000000, 0.000000000000000000, 0.000000000000000000 ) ) ;
#3925 = EDGE_CURVE ( 'NONE', #537, #4259, #2147, .T. ) ;
#3926 = CARTESIAN_POINT ( 'NONE',  ( -31.74999999999995737, 0.000000000000000000, 2.500000000000000888 ) ) ;
#3927 = CONICAL_SURFACE ( 'NONE', #1682, 2.099999999999997868, 1.029744258676653423 ) ;
#3928 = ORIENTED_EDGE ( 'NONE', *, *, #4446, .F. ) ;
#3929 = EDGE_LOOP ( 'NONE', ( #4638, #3367, #2943, #1276 ) ) ;
#3930 = AXIS2_PLACEMENT_3D ( 'NONE', #2, #1035, #1531 ) ;
#3931 = CIRCLE ( 'NONE', #1765, 1.535500000000000087 ) ;
#3932 = CARTESIAN_POINT ( 'NONE',  ( 15.00000000000000000, -16.00000000000000000, -28.64999999999999503 ) ) ;
#3933 = AXIS2_PLACEMENT_3D ( 'NONE', #4888, #4941, #3336 ) ;
#3934 = CIRCLE ( 'NONE', #3533, 23.00000000000000711 ) ;
#3935 = CARTESIAN_POINT ( 'NONE',  ( -31.74999999999995737, 0.000000000000000000, 3.500000000000000000 ) ) ;
#3936 = EDGE_LOOP ( 'NONE', ( #4011, #2285, #4117, #3141 ) ) ;
#3937 = ORIENTED_EDGE ( 'NONE', *, *, #2556, .T. ) ;
#3938 = VECTOR ( 'NONE', #368, 1000.000000000000000 ) ;
#3939 = VECTOR ( 'NONE', #4786, 1000.000000000000000 ) ;
#3940 = EDGE_CURVE ( 'NONE', #3640, #2138, #1783, .T. ) ;
#3941 = EDGE_CURVE ( 'NONE', #2143, #2727, #1068, .T. ) ;
#3942 = CARTESIAN_POINT ( 'NONE',  ( 5.200000000000002842, 0.000000000000000000, 0.000000000000000000 ) ) ;
#3943 = CARTESIAN_POINT ( 'NONE',  ( -6.708203932499367639, 2.000000000000000888, -20.00000000000000000 ) ) ;
#3944 = CARTESIAN_POINT ( 'NONE',  ( -15.26180729995793861, 15.99999999999999645, -26.00000000000000355 ) ) ;
#3945 = APPLICATION_CONTEXT ( 'automotive_design' ) ;
#3946 = ORIENTED_EDGE ( 'NONE', *, *, #3599, .T. ) ;
#3947 = AXIS2_PLACEMENT_3D ( 'NONE', #515, #4281, #3580 ) ;
#3948 = VERTEX_POINT ( 'NONE', #2598 ) ;
#3949 = DIRECTION ( 'NONE',  ( 0.000000000000000000, 0.000000000000000000, -1.000000000000000000 ) ) ;
#3950 = DIRECTION ( 'NONE',  ( -1.000000000000000000, 0.000000000000000000, 0.000000000000000000 ) ) ;
#3951 = FACE_BOUND ( 'NONE', #4354, .T. ) ;
#3952 = VECTOR ( 'NONE', #4485, 1000.000000000000000 ) ;
#3953 = ORIENTED_EDGE ( 'NONE', *, *, #4832, .T. ) ;
#3954 = DIRECTION ( 'NONE',  ( 1.000000000000000000, 0.000000000000000000, 0.000000000000000000 ) ) ;
#3955 = FACE_OUTER_BOUND ( 'NONE', #4601, .T. ) ;
#3956 = EDGE_LOOP ( 'NONE', ( #1153, #3440 ) ) ;
#3957 = CIRCLE ( 'NONE', #1870, 25.00000000000000000 ) ;
#3958 = ADVANCED_FACE ( 'NONE', ( #270 ), #2219, .T. ) ;
#3959 = CARTESIAN_POINT ( 'NONE',  ( -10.00000000000002132, 16.00000000000000000, -23.90000000000000568 ) ) ;
#3960 = FILL_AREA_STYLE ('',( #2440 ) ) ;
#3961 = CARTESIAN_POINT ( 'NONE',  ( -31.74999999999995737, 3.061616997868384127E-16, -2.500000000000000888 ) ) ;
#3962 = ORIENTED_EDGE ( 'NONE', *, *, #2053, .F. ) ;
#3963 = ORIENTED_EDGE ( 'NONE', *, *, #228, .F. ) ;
#3964 = DIRECTION ( 'NONE',  ( 1.000000000000000000, -0.000000000000000000, -0.000000000000000000 ) ) ;
#3965 = DIRECTION ( 'NONE',  ( 1.000000000000000000, -0.000000000000000000, -0.000000000000000000 ) ) ;
#3966 = DIRECTION ( 'NONE',  ( 0.000000000000000000, 0.000000000000000000, -1.000000000000000000 ) ) ;
#3967 = EDGE_CURVE ( 'NONE', #803, #3915, #2543, .T. ) ;
#3968 = ORIENTED_EDGE ( 'NONE', *, *, #3713, .F. ) ;
#3969 = EDGE_LOOP ( 'NONE', ( #729, #4820, #4301, #2630 ) ) ;
#3970 = CARTESIAN_POINT ( 'NONE',  ( -6.708203932499366751, -2.000000000000003553, -32.00000000000000000 ) ) ;
#3971 = CARTESIAN_POINT ( 'NONE',  ( -12.50000000000000000, -1.383461737289380927E-15, 4.000000000000000000 ) ) ;
#3972 = EDGE_CURVE ( 'NONE', #374, #2945, #1429, .T. ) ;
#3973 = EDGE_LOOP ( 'NONE', ( #785, #1998, #4951, #3482 ) ) ;
#3974 = DIRECTION ( 'NONE',  ( 1.000000000000000000, 0.000000000000000000, 0.000000000000000000 ) ) ;
#3975 = CARTESIAN_POINT ( 'NONE',  ( 8.500000000000001776, -9.407539813567788568E-16, 12.00000000000000000 ) ) ;
#3976 = VERTEX_POINT ( 'NONE', #1832 ) ;
#3977 =( NAMED_UNIT ( * ) PLANE_ANGLE_UNIT ( ) SI_UNIT ( $, .RADIAN. ) );
#3978 = CARTESIAN_POINT ( 'NONE',  ( 2.444036937190193033E-14, 6.999999999999999112, -32.00000000000000000 ) ) ;
#3979 = FACE_OUTER_BOUND ( 'NONE', #4423, .T. ) ;
#3980 = B_SPLINE_CURVE_WITH_KNOTS ( 'NONE', 3,
 ( #1534, #4265, #4594, #1192, #4208, #4233, #781, #3025, #1987, #2314, #807, #840, #472, #3514, #2464, #156 ),
 .UNSPECIFIED., .F., .F.,
 ( 4, 2, 2, 2, 2, 2, 2, 4 ),
 ( 0.000000000000000000, 0.0003092645584586379615, 0.0006185291169172759231, 0.0009277936753759138304, 0.001237058233834551846, 0.001546322792293189754, 0.001855587350751827661, 0.002474116467669114534 ),
 .UNSPECIFIED. ) ;
#3981 = COLOUR_RGB ( '', 0.66274510, 0.83137255, 0.94901961) ;
#3982 = ORIENTED_EDGE ( 'NONE', *, *, #4911, .T. ) ;
#3983 = EDGE_LOOP ( 'NONE', ( #2548, #2395, #1950, #4238, #435 ) ) ;
#3984 = CARTESIAN_POINT ( 'NONE',  ( 2.000000000000000000, 0.000000000000000000, 0.000000000000000000 ) ) ;
#3985 = ADVANCED_FACE ( 'NONE', ( #990 ), #2524, .T. ) ;
#3986 = DIRECTION ( 'NONE',  ( -1.000000000000000000, 0.000000000000000000, -0.000000000000000000 ) ) ;
#3987 = LINE ( 'NONE', #2775, #3856 ) ;
#3988 = VERTEX_POINT ( 'NONE', #2621 ) ;
#3989 = VERTEX_POINT ( 'NONE', #312 ) ;
#3990 = ADVANCED_FACE ( 'NONE', ( #1757 ), #3294, .F. ) ;
#3991 = CARTESIAN_POINT ( 'NONE',  ( 24.00000000000000000, 0.000000000000000000, 1.610000000000000098 ) ) ;
#3992 = FACE_OUTER_BOUND ( 'NONE', #3901, .T. ) ;
#3993 = VERTEX_POINT ( 'NONE', #4136 ) ;
#3994 = VECTOR ( 'NONE', #3668, 1000.000000000000000 ) ;
#3995 = LINE ( 'NONE', #145, #2805 ) ;
#3996 = EDGE_CURVE ( 'NONE', #1067, #2416, #2944, .T. ) ;
#3997 = LINE ( 'NONE', #2882, #3049 ) ;
#3998 = VECTOR ( 'NONE', #3697, 1000.000000000000000 ) ;
#3999 = ORIENTED_EDGE ( 'NONE', *, *, #3648, .F. ) ;
#4000 = VECTOR ( 'NONE', #2528, 1000.000000000000000 ) ;
#4001 = DIRECTION ( 'NONE',  ( 0.000000000000000000, 0.000000000000000000, -1.000000000000000000 ) ) ;
#4002 = CIRCLE ( 'NONE', #89, 2.041999999999999815 ) ;
#4003 = VERTEX_POINT ( 'NONE', #2239 ) ;
#4004 = VECTOR ( 'NONE', #806, 1000.000000000000000 ) ;
#4005 = FACE_OUTER_BOUND ( 'NONE', #4906, .T. ) ;
#4006 = DIRECTION ( 'NONE',  ( 1.106769389831504189E-16, 1.000000000000000000, 0.000000000000000000 ) ) ;
#4007 = CARTESIAN_POINT ( 'NONE',  ( 0.000000000000000000, 25.00000000000000000, -20.00000000000000000 ) ) ;
#4008 = AXIS2_PLACEMENT_3D ( 'NONE', #4431, #2446, #3264 ) ;
#4009 = AXIS2_PLACEMENT_3D ( 'NONE', #3192, #884, #1286 ) ;
#4010 = ORIENTED_EDGE ( 'NONE', *, *, #1316, .F. ) ;
#4011 = ORIENTED_EDGE ( 'NONE', *, *, #3560, .T. ) ;
#4012 = SURFACE_STYLE_USAGE ( .BOTH. , #3712 ) ;
#4013 = CIRCLE ( 'NONE', #2747, 22.99999999999998934 ) ;
#4014 = LINE ( 'NONE', #3991, #1552 ) ;
#4015 = VECTOR ( 'NONE', #87, 1000.000000000000000 ) ;
#4016 = DIRECTION ( 'NONE',  ( 1.106769389831504313E-16, -1.000000000000000000, 0.000000000000000000 ) ) ;
#4017 = ORIENTED_EDGE ( 'NONE', *, *, #3019, .F. ) ;
#4018 = DIRECTION ( 'NONE',  ( -1.000000000000000000, -0.000000000000000000, -0.000000000000000000 ) ) ;
#4019 = ORIENTED_EDGE ( 'NONE', *, *, #3996, .T. ) ;
#4020 = VECTOR ( 'NONE', #1854, 1000.000000000000000 ) ;
#4021 = DIRECTION ( 'NONE',  ( 0.000000000000000000, 0.000000000000000000, -1.000000000000000000 ) ) ;
#4022 = LINE ( 'NONE', #3975, #3362 ) ;
#4023 = VERTEX_POINT ( 'NONE', #3761 ) ;
#4024 = EDGE_CURVE ( 'NONE', #4850, #340, #829, .T. ) ;
#4025 = EDGE_CURVE ( 'NONE', #374, #2945, #585, .T. ) ;
#4026 = ADVANCED_FACE ( 'NONE', ( #1460 ), #2172, .F. ) ;
#4027 = CARTESIAN_POINT ( 'NONE',  ( 1.387778780781444295E-15, 4.108768631691174362E-15, -12.00000000000000000 ) ) ;
#4028 = APPLICATION_PROTOCOL_DEFINITION ( 'draft international standard', 'automotive_design', 1998, #609 ) ;
#4029 = ORIENTED_EDGE ( 'NONE', *, *, #3058, .F. ) ;
#4030 = EDGE_CURVE ( 'NONE', #3847, #3989, #28, .T. ) ;
#4031 = AXIS2_PLACEMENT_3D ( 'NONE', #2670, #2789, #2844 ) ;
#4032 = DIRECTION ( 'NONE',  ( -3.578554360455197734E-15, -1.000000000000000000, 0.000000000000000000 ) ) ;
#4033 = PLANE ( 'NONE',  #505 ) ;
#4034 = CARTESIAN_POINT ( 'NONE',  ( 22.40016391766193138, -11.10102051443364424, -20.00000000000000000 ) ) ;
#4035 = ORIENTED_EDGE ( 'NONE', *, *, #2983, .F. ) ;
#4036 = EDGE_LOOP ( 'NONE', ( #4010, #2583, #1914, #903, #3190, #1567, #4702, #509, #4227, #4408 ) ) ;
#4037 = LINE ( 'NONE', #4347, #1129 ) ;
#4038 = DIRECTION ( 'NONE',  ( 0.000000000000000000, 0.000000000000000000, 1.000000000000000000 ) ) ;
#4039 = EDGE_CURVE ( 'NONE', #1680, #4479, #733, .T. ) ;
#4040 = CARTESIAN_POINT ( 'NONE',  ( 0.000000000000000000, 0.000000000000000000, -20.00000000000000000 ) ) ;
#4041 = ORIENTED_EDGE ( 'NONE', *, *, #4580, .T. ) ;
#4042 = CARTESIAN_POINT ( 'NONE',  ( 6.497531322021036645E-14, -16.00000000000000000, -26.00000000000000355 ) ) ;
#4043 = FACE_BOUND ( 'NONE', #4773, .T. ) ;
#4044 = DIRECTION ( 'NONE',  ( 1.000000000000000000, -0.000000000000000000, -0.000000000000000000 ) ) ;
#4045 = EDGE_CURVE ( 'NONE', #392, #2206, #2267, .T. ) ;
#4046 = ORIENTED_EDGE ( 'NONE', *, *, #2556, .F. ) ;
#4047 = FACE_OUTER_BOUND ( 'NONE', #911, .T. ) ;
#4048 = CARTESIAN_POINT ( 'NONE',  ( 2.000000000000000000, 0.000000000000000000, 0.000000000000000000 ) ) ;
#4049 = APPLICATION_PROTOCOL_DEFINITION ( 'draft international standard', 'automotive_design', 1998, #4189 ) ;
#4050 = SURFACE_STYLE_USAGE ( .BOTH. , #1743 ) ;
#4051 = EDGE_CURVE ( 'NONE', #1518, #1504, #1966, .T. ) ;
#4052 = VERTEX_POINT ( 'NONE', #2674 ) ;
#4053 = CARTESIAN_POINT ( 'NONE',  ( -4.473192950568998942E-14, -12.50000000000000178, -12.00000000000000000 ) ) ;
#4054 = ADVANCED_FACE ( 'NONE', ( #4950 ), #2843, .T. ) ;
#4055 =( GEOMETRIC_REPRESENTATION_CONTEXT ( 3 ) GLOBAL_UNCERTAINTY_ASSIGNED_CONTEXT ( ( #4245 ) ) GLOBAL_UNIT_ASSIGNED_CONTEXT ( ( #4539, #2468, #3893 ) ) REPRESENTATION_CONTEXT ( 'NONE', 'WORKASPACE' ) );
#4056 = CARTESIAN_POINT ( 'NONE',  ( 2.302289838212012812E-14, -16.00000000000000000, -28.09999999999999432 ) ) ;
#4057 = LINE ( 'NONE', #4079, #1621 ) ;
#4058 = ORIENTED_EDGE ( 'NONE', *, *, #4955, .F. ) ;
#4059 = ORIENTED_EDGE ( 'NONE', *, *, #1478, .F. ) ;
#4060 = CARTESIAN_POINT ( 'NONE',  ( -23.68543856465402442, -8.000000000000003553, -4.000000000000000000 ) ) ;
#4061 = CARTESIAN_POINT ( 'NONE',  ( 22.21307774062918128, 11.47223234890555688, -20.05227268063044832 ) ) ;
#4062 = DIRECTION ( 'NONE',  ( 0.000000000000000000, 0.000000000000000000, 1.000000000000000000 ) ) ;
#4063 = VERTEX_POINT ( 'NONE', #3493 ) ;
#4064 = PRODUCT_DEFINITION_FORMATION_WITH_SPECIFIED_SOURCE ( 'ANY', '', #1016, .NOT_KNOWN. ) ;
#4065 = LINE ( 'NONE', #2129, #796 ) ;
#4066 = DIRECTION ( 'NONE',  ( 0.000000000000000000, -1.000000000000000000, 9.783878858594330870E-16 ) ) ;
#4067 = VECTOR ( 'NONE', #4494, 1000.000000000000000 ) ;
#4068 = ORIENTED_EDGE ( 'NONE', *, *, #2316, .F. ) ;
#4069 = ADVANCED_FACE ( 'NONE', ( #3078, #58 ), #4534, .F. ) ;
#4070 = CARTESIAN_POINT ( 'NONE',  ( -9.000000000000001776, 2.000000000000000000, -32.00000000000000000 ) ) ;
#4071 = VECTOR ( 'NONE', #1093, 1000.000000000000000 ) ;
#4072 = PLANE ( 'NONE',  #4918 ) ;
#4073 = VERTEX_POINT ( 'NONE', #1112 ) ;
#4074 = AXIS2_PLACEMENT_3D ( 'NONE', #4931, #346, #669 ) ;
#4075 = ADVANCED_FACE ( 'Placement Plane', ( #34, #2371 ), #1584, .F. ) ;
#4076 = CARTESIAN_POINT ( 'NONE',  ( 22.61674500023158885, 10.65336738338371880, -23.26995442300275130 ) ) ;
#4077 = AXIS2_PLACEMENT_3D ( 'NONE', #1171, #419, #3518 ) ;
#4078 = FACE_OUTER_BOUND ( 'NONE', #1493, .T. ) ;
#4079 = CARTESIAN_POINT ( 'NONE',  ( 25.00000000000000000, 0.000000000000000000, 2.055000000000000160 ) ) ;
#4080 = VERTEX_POINT ( 'NONE', #366 ) ;
#4081 = EDGE_CURVE ( 'NONE', #2811, #4838, #159, .T. ) ;
#4082 = CIRCLE ( 'NONE', #254, 25.00000000000000000 ) ;
#4083 = EDGE_CURVE ( 'NONE', #3410, #811, #3466, .T. ) ;
#4084 = DIRECTION ( 'NONE',  ( 1.000000000000000000, 0.000000000000000000, -0.000000000000000000 ) ) ;
#4085 =( NAMED_UNIT ( * ) SI_UNIT ( $, .STERADIAN. ) SOLID_ANGLE_UNIT ( ) );
#4086 = DIRECTION ( 'NONE',  ( 1.000000000000000000, -1.892318758829013864E-15, 0.000000000000000000 ) ) ;
#4087 = LINE ( 'NONE', #683, #3057 ) ;
#4088 = CIRCLE ( 'NONE', #4484, 6.999999999999999112 ) ;
#4089 = ORIENTED_EDGE ( 'NONE', *, *, #3967, .F. ) ;
#4090 = DIRECTION ( 'NONE',  ( 0.000000000000000000, 1.000000000000000000, -9.783878858594330870E-16 ) ) ;
#4091 = ORIENTED_EDGE ( 'NONE', *, *, #4886, .T. ) ;
#4092 = ORIENTED_EDGE ( 'NONE', *, *, #4830, .F. ) ;
#4093 = AXIS2_PLACEMENT_3D ( 'NONE', #1793, #3764, #4952 ) ;
#4094 = VECTOR ( 'NONE', #3314, 1000.000000000000000 ) ;
#4095 = CIRCLE ( 'NONE', #1941, 3.299999999999999822 ) ;
#4096 = DIRECTION ( 'NONE',  ( 1.000000000000000000, 1.357798298438996130E-15, 0.000000000000000000 ) ) ;
#4097 = DIRECTION ( 'NONE',  ( -1.000000000000000000, 0.000000000000000000, 0.000000000000000000 ) ) ;
#4098 = FACE_OUTER_BOUND ( 'NONE', #2793, .T. ) ;
#4099 = VECTOR ( 'NONE', #2323, 1000.000000000000114 ) ;
#4100 = CIRCLE ( 'NONE', #3233, 0.2000000000000000944 ) ;
#4101 = ORIENTED_EDGE ( 'NONE', *, *, #2261, .T. ) ;
#4102 = CARTESIAN_POINT ( 'NONE',  ( 0.000000000000000000, 0.000000000000000000, -20.00000000000000000 ) ) ;
#4103 = AXIS2_PLACEMENT_3D ( 'NONE', #3366, #4896, #4826 ) ;
#4104 = CARTESIAN_POINT ( 'NONE',  ( 3.999999999999999112, 0.000000000000000000, 0.000000000000000000 ) ) ;
#4105 = EDGE_LOOP ( 'NONE', ( #4428, #1792, #1375, #2704 ) ) ;
#4106 = VECTOR ( 'NONE', #2718, 1000.000000000000000 ) ;
#4107 = FACE_OUTER_BOUND ( 'NONE', #3732, .T. ) ;
#4108 = CARTESIAN_POINT ( 'NONE',  ( 0.000000000000000000, 0.000000000000000000, -12.00000000000000000 ) ) ;
#4109 = CARTESIAN_POINT ( 'NONE',  ( 0.000000000000000000, 0.000000000000000000, 0.000000000000000000 ) ) ;
#4110 = EDGE_LOOP ( 'NONE', ( #530, #3503, #2329 ) ) ;
#4111 = AXIS2_PLACEMENT_3D ( 'NONE', #2480, #4001, #4397 ) ;
#4112 = EDGE_LOOP ( 'NONE', ( #1828, #2489, #3218, #2553 ) ) ;
#4113 = DIRECTION ( 'NONE',  ( -1.000000000000000000, 0.000000000000000000, 0.000000000000000000 ) ) ;
#4114 = DIRECTION ( 'NONE',  ( -0.000000000000000000, -0.000000000000000000, 1.000000000000000000 ) ) ;
#4115 = CARTESIAN_POINT ( 'NONE',  ( 2.000000000000000000, -0.8865213383406690406, 1.535500000000000975 ) ) ;
#4116 = EDGE_CURVE ( 'NONE', #4310, #3217, #3980, .T. ) ;
#4117 = ORIENTED_EDGE ( 'NONE', *, *, #450, .F. ) ;
#4118 = LINE ( 'NONE', #4489, #426 ) ;
#4119 = CARTESIAN_POINT ( 'NONE',  ( 0.000000000000000000, 0.000000000000000000, -12.00000000000000000 ) ) ;
#4120 = CARTESIAN_POINT ( 'NONE',  ( 0.000000000000000000, 0.000000000000000000, 4.000000000000000000 ) ) ;
#4121 = ADVANCED_FACE ( 'NONE', ( #958 ), #1684, .T. ) ;
#4122 = VERTEX_POINT ( 'NONE', #4385 ) ;
#4123 = CARTESIAN_POINT ( 'NONE',  ( 5.000000000000002665, 0.000000000000000000, -2.700000000000001066 ) ) ;
#4124 = DIRECTION ( 'NONE',  ( 2.168404344971009361E-16, -1.000000000000000000, 0.000000000000000000 ) ) ;
#4125 = CARTESIAN_POINT ( 'NONE',  ( 0.000000000000000000, 0.000000000000000000, -4.000000000000000000 ) ) ;
#4126 = ORIENTED_EDGE ( 'NONE', *, *, #880, .F. ) ;
#4127 = DIRECTION ( 'NONE',  ( 0.000000000000000000, 0.000000000000000000, 1.000000000000000000 ) ) ;
#4128 = CARTESIAN_POINT ( 'NONE',  ( 0.000000000000000000, 0.000000000000000000, -32.00000000000000000 ) ) ;
#4129 = DIRECTION ( 'NONE',  ( 0.000000000000000000, 0.4999999999999993339, -0.8660254037844390407 ) ) ;
#4130 = CARTESIAN_POINT ( 'NONE',  ( -13.99999999999993250, -16.00000000000000000, -23.90000000000000568 ) ) ;
#4131 = VERTEX_POINT ( 'NONE', #3944 ) ;
#4132 = EDGE_LOOP ( 'NONE', ( #3056, #4468, #3188, #4961 ) ) ;
#4133 = SURFACE_STYLE_FILL_AREA ( #2288 ) ;
#4134 = CARTESIAN_POINT ( 'NONE',  ( -21.37171027316253102, -8.499999999999925393, -4.000000000000000000 ) ) ;
#4135 = CARTESIAN_POINT ( 'NONE',  ( 5.200000000000002842, 3.306546357697854719E-16, 2.700000000000001066 ) ) ;
#4136 = CARTESIAN_POINT ( 'NONE',  ( 23.68543856465402797, 7.999999999999996447, -4.000000000000000000 ) ) ;
#4137 = ORIENTED_EDGE ( 'NONE', *, *, #3972, .F. ) ;
#4138 =( GEOMETRIC_REPRESENTATION_CONTEXT ( 3 ) GLOBAL_UNCERTAINTY_ASSIGNED_CONTEXT ( ( #2356 ) ) GLOBAL_UNIT_ASSIGNED_CONTEXT ( ( #630, #265, #1810 ) ) REPRESENTATION_CONTEXT ( 'NONE', 'WORKASPACE' ) );
#4139 = ORIENTED_EDGE ( 'NONE', *, *, #3967, .T. ) ;
#4140 = DIRECTION ( 'NONE',  ( -1.000000000000000000, -0.000000000000000000, 0.000000000000000000 ) ) ;
#4141 = EDGE_CURVE ( 'NONE', #2569, #181, #4570, .T. ) ;
#4142 = EDGE_CURVE ( 'NONE', #2765, #1262, #4342, .T. ) ;
#4143 = DIRECTION ( 'NONE',  ( -1.000000000000000000, 0.000000000000000000, 0.000000000000000000 ) ) ;
#4144 = ORIENTED_EDGE ( 'NONE', *, *, #379, .T. ) ;
#4145 = ADVANCED_FACE ( 'NONE', ( #2068 ), #4667, .F. ) ;
#4146 = ADVANCED_FACE ( 'NONE', ( #1289 ), #4287, .T. ) ;
#4147 = CARTESIAN_POINT ( 'NONE',  ( 0.000000000000000000, 0.000000000000000000, -4.000000000000000000 ) ) ;
#4148 = ORIENTED_EDGE ( 'NONE', *, *, #2161, .T. ) ;
#4149 = AXIS2_PLACEMENT_3D ( 'NONE', #642, #4518, #2249 ) ;
#4150 = CARTESIAN_POINT ( 'NONE',  ( 22.18526740102421257, 11.52862861652371507, -21.98103133599976289 ) ) ;
#4151 = DIRECTION ( 'NONE',  ( -0.000000000000000000, -0.000000000000000000, -1.000000000000000000 ) ) ;
#4152 = CARTESIAN_POINT ( 'NONE',  ( 3.999999999999997335, 0.000000000000000000, -2.200000000000001066 ) ) ;
#4153 = DIRECTION ( 'NONE',  ( -0.9474175425861609545, 0.3199999999999996181, 0.000000000000000000 ) ) ;
#4154 = ORIENTED_EDGE ( 'NONE', *, *, #3181, .F. ) ;
#4155 = VECTOR ( 'NONE', #4727, 1000.000000000000000 ) ;
#4156 = LINE ( 'NONE', #2636, #836 ) ;
#4157 = DIRECTION ( 'NONE',  ( 0.000000000000000000, 1.224646799147353207E-16, 1.000000000000000000 ) ) ;
#4158 = DIRECTION ( 'NONE',  ( 1.000000000000000000, 2.168404344971009361E-16, 0.000000000000000000 ) ) ;
#4159 = DIRECTION ( 'NONE',  ( -1.000000000000000000, 0.000000000000000000, 0.000000000000000000 ) ) ;
#4160 = EDGE_CURVE ( 'NONE', #3165, #2165, #3987, .T. ) ;
#4161 = VECTOR ( 'NONE', #1616, 999.9999999999998863 ) ;
#4162 = ORIENTED_EDGE ( 'NONE', *, *, #4704, .F. ) ;
#4163 = DIRECTION ( 'NONE',  ( -0.000000000000000000, -0.000000000000000000, 1.000000000000000000 ) ) ;
#4164 = AXIS2_PLACEMENT_3D ( 'NONE', #1317, #2854, #3285 ) ;
#4165 = DIRECTION ( 'NONE',  ( 1.106769389831504313E-16, -1.000000000000000000, 0.000000000000000000 ) ) ;
#4166 = AXIS2_PLACEMENT_3D ( 'NONE', #3045, #1406, #1861 ) ;
#4167 = ORIENTED_EDGE ( 'NONE', *, *, #848, .F. ) ;
#4168 = AXIS2_PLACEMENT_3D ( 'NONE', #1379, #3563, #2515 ) ;
#4169 = PLANE ( 'NONE',  #76 ) ;
#4170 = DIRECTION ( 'NONE',  ( 0.000000000000000000, -0.5000000000000011102, -0.8660254037844379305 ) ) ;
#4171 = AXIS2_PLACEMENT_3D ( 'NONE', #4478, #1781, #210 ) ;
#4172 = EDGE_CURVE ( 'NONE', #7, #3027, #3194, .T. ) ;
#4173 = EDGE_CURVE ( 'NONE', #4655, #1319, #937, .T. ) ;
#4174 = EDGE_CURVE ( 'NONE', #121, #4122, #1244, .T. ) ;
#4175 = VERTEX_POINT ( 'NONE', #4715 ) ;
#4176 = AXIS2_PLACEMENT_3D ( 'NONE', #2136, #3240, #252 ) ;
#4177 = CARTESIAN_POINT ( 'NONE',  ( 0.2500000000000002220, 0.000000000000000000, 4.250000000000000000 ) ) ;
#4178 = CARTESIAN_POINT ( 'NONE',  ( 0.000000000000000000, 0.000000000000000000, -20.00000000000000000 ) ) ;
#4179 = CARTESIAN_POINT ( 'NONE',  ( 24.55500000000002103, 0.000000000000000000, 2.500000000000001332 ) ) ;
#4180 = DIRECTION ( 'NONE',  ( -0.000000000000000000, 1.000000000000000000, -0.000000000000000000 ) ) ;
#4181 = EDGE_CURVE ( 'NONE', #497, #2491, #863, .T. ) ;
#4182 = VERTEX_POINT ( 'NONE', #4772 ) ;
#4183 = LINE ( 'NONE', #3932, #4837 ) ;
#4184 =( LENGTH_UNIT ( ) NAMED_UNIT ( * ) SI_UNIT ( .MILLI., .METRE. ) );
#4185 = DIRECTION ( 'NONE',  ( -1.000000000000000000, -0.000000000000000000, -0.000000000000000000 ) ) ;
#4186 = FACE_OUTER_BOUND ( 'NONE', #1455, .T. ) ;
#4187 = CARTESIAN_POINT ( 'NONE',  ( 22.17126811103361206, 11.55175229948174120, -31.89759920908706547 ) ) ;
#4188 = ORIENTED_EDGE ( 'NONE', *, *, #898, .F. ) ;
#4189 = APPLICATION_CONTEXT ( 'automotive_design' ) ;
#4190 = ORIENTED_EDGE ( 'NONE', *, *, #2003, .F. ) ;
#4191 = SURFACE_SIDE_STYLE ('',( #1507 ) ) ;
#4192 = LINE ( 'NONE', #3421, #1212 ) ;
#4193 = ORIENTED_EDGE ( 'NONE', *, *, #3925, .T. ) ;
#4194 = DIRECTION ( 'NONE',  ( -1.000000000000000000, -0.000000000000000000, -0.000000000000000000 ) ) ;
#4195 = DIRECTION ( 'NONE',  ( -0.000000000000000000, 0.000000000000000000, 1.000000000000000000 ) ) ;
#4196 = ADVANCED_FACE ( 'NONE', ( #1336 ), #496, .F. ) ;
#4197 = ORIENTED_EDGE ( 'NONE', *, *, #2161, .F. ) ;
#4198 = VERTEX_POINT ( 'NONE', #2873 ) ;
#4199 = DIRECTION ( 'NONE',  ( -4.336808689942018722E-16, -1.000000000000000000, 0.000000000000000000 ) ) ;
#4200 = CARTESIAN_POINT ( 'NONE',  ( 19.30673457630784995, 12.49999999999993783, -12.00000000000000000 ) ) ;
#4201 = DIRECTION ( 'NONE',  ( 0.000000000000000000, 0.000000000000000000, -1.000000000000000000 ) ) ;
#4202 = DIRECTION ( 'NONE',  ( -0.3200000000000010614, -0.9474175425861606215, 0.000000000000000000 ) ) ;
#4203 = ORIENTED_EDGE ( 'NONE', *, *, #1903, .T. ) ;
#4204 = EDGE_CURVE ( 'NONE', #4243, #2345, #4741, .T. ) ;
#4205 = FACE_OUTER_BOUND ( 'NONE', #4273, .T. ) ;
#4206 = CARTESIAN_POINT ( 'NONE',  ( -4.336808689942023652E-16, 2.000000000000002220, -12.00000000000000000 ) ) ;
#4207 = DIRECTION ( 'NONE',  ( 1.000000000000000000, 0.000000000000000000, 0.000000000000000000 ) ) ;
#4208 = CARTESIAN_POINT ( 'NONE',  ( 22.17126811103361206, -11.55175229948174476, -20.10240079091293808 ) ) ;
#4209 = ORIENTED_EDGE ( 'NONE', *, *, #1551, .F. ) ;
#4210 = ORIENTED_EDGE ( 'NONE', *, *, #3573, .T. ) ;
#4211 = DIRECTION ( 'NONE',  ( 1.000000000000000000, 3.552713678800500929E-15, 0.000000000000000000 ) ) ;
#4212 = DIRECTION ( 'NONE',  ( -0.000000000000000000, -0.000000000000000000, 1.000000000000000000 ) ) ;
#4213 = FACE_OUTER_BOUND ( 'NONE', #1133, .T. ) ;
#4214 = ORIENTED_EDGE ( 'NONE', *, *, #4608, .T. ) ;
#4215 = AXIS2_PLACEMENT_3D ( 'NONE', #1936, #334, #1189 ) ;
#4216 = CARTESIAN_POINT ( 'NONE',  ( 6.999999999999999112, 0.000000000000000000, -20.00000000000000000 ) ) ;
#4217 = FILL_AREA_STYLE ('',( #1152 ) ) ;
#4218 = VERTEX_POINT ( 'NONE', #1608 ) ;
#4219 = VERTEX_POINT ( 'NONE', #4007 ) ;
#4220 = EDGE_CURVE ( 'NONE', #2220, #1467, #3177, .T. ) ;
#4221 = SHAPE_REPRESENTATION ( 'locker', ( #1918 ), #1581 ) ;
#4222 = CARTESIAN_POINT ( 'NONE',  ( 22.82142399877221450, -10.20738559227135944, -27.61557768215598685 ) ) ;
#4223 = CARTESIAN_POINT ( 'NONE',  ( 2.172477277502393807E-14, -16.00000000000000000, -26.00000000000000355 ) ) ;
#4224 = FACE_OUTER_BOUND ( 'NONE', #2246, .T. ) ;
#4225 = LINE ( 'NONE', #4942, #2666 ) ;
#4226 = VECTOR ( 'NONE', #694, 1000.000000000000000 ) ;
#4227 = ORIENTED_EDGE ( 'NONE', *, *, #462, .F. ) ;
#4228 = EDGE_CURVE ( 'NONE', #3976, #4198, #2016, .T. ) ;
#4229 = DIRECTION ( 'NONE',  ( -1.000000000000000000, 0.000000000000000000, -6.982962677686266711E-15 ) ) ;
#4230 = STYLED_ITEM ( 'NONE', ( #1587 ), #38 ) ;
#4231 = DIRECTION ( 'NONE',  ( -0.000000000000000000, -0.000000000000000000, -1.000000000000000000 ) ) ;
#4232 = DIRECTION ( 'NONE',  ( -1.000000000000000000, -0.000000000000000000, -0.000000000000000000 ) ) ;
#4233 = CARTESIAN_POINT ( 'NONE',  ( 22.08746549892785893, -11.71119031839158176, -20.20216775413354426 ) ) ;
#4234 = ADVANCED_FACE ( 'NONE', ( #4315 ), #2421, .T. ) ;
#4235 = EDGE_CURVE ( 'NONE', #4410, #4738, #984, .T. ) ;
#4236 = ORIENTED_EDGE ( 'NONE', *, *, #1602, .T. ) ;
#4237 = CIRCLE ( 'NONE', #83, 2.099999999999997868 ) ;
#4238 = ORIENTED_EDGE ( 'NONE', *, *, #4045, .T. ) ;
#4239 = CARTESIAN_POINT ( 'NONE',  ( -14.00000000000006395, 16.00000000000000000, -23.90000000000000568 ) ) ;
#4240 = CARTESIAN_POINT ( 'NONE',  ( 0.000000000000000000, 0.000000000000000000, 12.00000000000000000 ) ) ;
#4241 = CARTESIAN_POINT ( 'NONE',  ( 22.99999999999998934, 0.000000000000000000, -4.000000000000000000 ) ) ;
#4242 = VECTOR ( 'NONE', #2701, 1000.000000000000000 ) ;
#4243 = VERTEX_POINT ( 'NONE', #650 ) ;
#4244 = CIRCLE ( 'NONE', #572, 0.2000000000000000944 ) ;
#4245 = UNCERTAINTY_MEASURE_WITH_UNIT (LENGTH_MEASURE( 1.000000000000000082E-05 ), #4539, 'distance_accuracy_value', 'NONE');
#4246 = PRODUCT_DEFINITION_SHAPE ( 'NONE', 'NONE',  #2307 ) ;
#4247 = CARTESIAN_POINT ( 'NONE',  ( 0.000000000000000000, -1.178949249685213863, 2.042000000000002924 ) ) ;
#4248 = ORIENTED_EDGE ( 'NONE', *, *, #362, .T. ) ;
#4249 = AXIS2_PLACEMENT_3D ( 'NONE', #2388, #4282, #833 ) ;
#4250 = CIRCLE ( 'NONE', #4009, 25.00000000000000000 ) ;
#4251 = ORIENTED_EDGE ( 'NONE', *, *, #2400, .F. ) ;
#4252 = CIRCLE ( 'NONE', #4093, 2.000000000000000444 ) ;
#4253 = VECTOR ( 'NONE', #359, 1000.000000000000000 ) ;
#4254 = CIRCLE ( 'NONE', #184, 25.00000000000000000 ) ;
#4255 = CYLINDRICAL_SURFACE ( 'NONE', #432, 6.999999999999999112 ) ;
#4256 = LINE ( 'NONE', #3457, #1444 ) ;
#4257 = ORIENTED_EDGE ( 'NONE', *, *, #4729, .F. ) ;
#4258 = CIRCLE ( 'NONE', #1230, 1.000000000000000888 ) ;
#4259 = VERTEX_POINT ( 'NONE', #1451 ) ;
#4260 = PRODUCT_CONTEXT ( 'NONE', #938, 'mechanical' ) ;
#4261 = EDGE_CURVE ( 'NONE', #2220, #4937, #626, .T. ) ;
#4262 = LINE ( 'NONE', #838, #92 ) ;
#4263 = EDGE_CURVE ( 'NONE', #3692, #3812, #2891, .T. ) ;
#4264 = DIRECTION ( 'NONE',  ( 0.000000000000000000, 0.000000000000000000, 1.000000000000000000 ) ) ;
#4265 = CARTESIAN_POINT ( 'NONE',  ( 22.35373982437574014, -11.19469724424307344, -20.00000000000000355 ) ) ;
#4266 = VERTEX_POINT ( 'NONE', #1382 ) ;
#4267 = CLOSED_SHELL ( 'NONE', ( #2093, #719, #1508, #4512, #4339, #4731, #1445, #4812, #3378, #2907, #3349, #381, #4920, #3031, #1846, #4919, #2592, #2252, #295, #4234, #2280, #2658 ) ) ;
#4268 = ORIENTED_EDGE ( 'NONE', *, *, #1669, .T. ) ;
#4269 = DIRECTION ( 'NONE',  ( 0.000000000000000000, 0.000000000000000000, -1.000000000000000000 ) ) ;
#4270 = CARTESIAN_POINT ( 'NONE',  ( 0.000000000000000000, 0.000000000000000000, -20.00000000000000000 ) ) ;
#4271 = CIRCLE ( 'NONE', #2043, 3.299999999999999822 ) ;
#4272 = CARTESIAN_POINT ( 'NONE',  ( 0.000000000000000000, 0.000000000000000000, -4.000000000000000000 ) ) ;
#4273 = EDGE_LOOP ( 'NONE', ( #1486, #1579, #1517 ) ) ;
#4274 = VECTOR ( 'NONE', #3626, 1000.000000000000000 ) ;
#4275 = CARTESIAN_POINT ( 'NONE',  ( 0.000000000000000000, 0.000000000000000000, -20.00000000000000000 ) ) ;
#4276 = EDGE_CURVE ( 'NONE', #1179, #2929, #4057, .T. ) ;
#4277 = CARTESIAN_POINT ( 'NONE',  ( 0.000000000000000000, 25.00000000000000000, -32.00000000000000000 ) ) ;
#4278 = EDGE_LOOP ( 'NONE', ( #2934, #3454, #926 ) ) ;
#4279 = VERTEX_POINT ( 'NONE', #231 ) ;
#4280 = LINE ( 'NONE', #3092, #1222 ) ;
#4281 = DIRECTION ( 'NONE',  ( -1.000000000000000000, -0.000000000000000000, -0.000000000000000000 ) ) ;
#4282 = DIRECTION ( 'NONE',  ( -1.000000000000000000, -0.000000000000000000, 0.000000000000000000 ) ) ;
#4283 = EDGE_LOOP ( 'NONE', ( #4137, #3738 ) ) ;
#4284 = ORIENTED_EDGE ( 'NONE', *, *, #1316, .T. ) ;
#4285 = DIRECTION ( 'NONE',  ( 1.000000000000000000, 0.000000000000000000, 0.000000000000000000 ) ) ;
#4286 = LINE ( 'NONE', #1635, #2735 ) ;
#4287 = PLANE ( 'NONE',  #579 ) ;
#4288 = APPLICATION_CONTEXT ( 'automotive_design' ) ;
#4289 = ORIENTED_EDGE ( 'NONE', *, *, #3269, .F. ) ;
#4290 = ADVANCED_FACE ( 'NONE', ( #2560, #1352 ), #1056, .T. ) ;
#4291 = ORIENTED_EDGE ( 'NONE', *, *, #4767, .T. ) ;
#4292 = FILL_AREA_STYLE ('',( #2397 ) ) ;
#4293 = DIRECTION ( 'NONE',  ( 1.000000000000000000, 0.000000000000000000, 0.000000000000000000 ) ) ;
#4294 = DIRECTION ( 'NONE',  ( -0.000000000000000000, 0.000000000000000000, 1.000000000000000000 ) ) ;
#4295 = DIRECTION ( 'NONE',  ( 1.000000000000000000, 0.000000000000000000, 0.000000000000000000 ) ) ;
#4296 = VERTEX_POINT ( 'NONE', #1807 ) ;
#4297 = PRODUCT_RELATED_PRODUCT_CATEGORY ( 'part', '', ( #1016 ) ) ;
#4298 = EDGE_CURVE ( 'NONE', #1595, #297, #2965, .T. ) ;
#4299 = LINE ( 'NONE', #4778, #3203 ) ;
#4300 = CARTESIAN_POINT ( 'NONE',  ( 2.500000000000000000, 2.357898499370433054, -1.951563910473907981E-15 ) ) ;
#4301 = ORIENTED_EDGE ( 'NONE', *, *, #4039, .F. ) ;
#4302 = ORIENTED_EDGE ( 'NONE', *, *, #3540, .F. ) ;
#4303 = EDGE_CURVE ( 'NONE', #3657, #586, #427, .T. ) ;
#4304 = COLOUR_RGB ( '', 0.72549020, 0.75294118, 0.79215686) ;
#4305 = ADVANCED_FACE ( 'NONE', ( #2517 ), #4487, .F. ) ;
#4306 = FACE_OUTER_BOUND ( 'NONE', #2914, .T. ) ;
#4307 = PRESENTATION_STYLE_ASSIGNMENT (( #3579 ) ) ;
#4308 = DIRECTION ( 'NONE',  ( -0.000000000000000000, 0.000000000000000000, 1.000000000000000000 ) ) ;
#4309 = DIRECTION ( 'NONE',  ( -1.000000000000000000, -0.000000000000000000, -0.000000000000000000 ) ) ;
#4310 = VERTEX_POINT ( 'NONE', #4034 ) ;
#4311 = VERTEX_POINT ( 'NONE', #678 ) ;
#4312 = LINE ( 'NONE', #2014, #2497 ) ;
#4313 = CYLINDRICAL_SURFACE ( 'NONE', #21, 1.000000000000000888 ) ;
#4314 = CIRCLE ( 'NONE', #1118, 17.00000000000000000 ) ;
#4315 = FACE_OUTER_BOUND ( 'NONE', #1539, .T. ) ;
#4316 = ORIENTED_EDGE ( 'NONE', *, *, #2626, .T. ) ;
#4317 = CIRCLE ( 'NONE', #1284, 17.00000000000000000 ) ;
#4318 = EDGE_LOOP ( 'NONE', ( #3883, #3635, #3197, #1601, #1944 ) ) ;
#4319 = CARTESIAN_POINT ( 'NONE',  ( 16.10609822396473945, -5.439999999999995062, -12.00000000000000000 ) ) ;
#4320 = DIRECTION ( 'NONE',  ( 0.000000000000000000, 0.000000000000000000, 1.000000000000000000 ) ) ;
#4321 = DIRECTION ( 'NONE',  ( -4.336808689942018722E-16, -1.000000000000000000, 0.000000000000000000 ) ) ;
#4322 = CIRCLE ( 'NONE', #1600, 2.000000000000000444 ) ;
#4323 = ORIENTED_EDGE ( 'NONE', *, *, #322, .T. ) ;
#4324 = DIRECTION ( 'NONE',  ( 0.000000000000000000, 0.000000000000000000, -1.000000000000000000 ) ) ;
#4325 = FACE_OUTER_BOUND ( 'NONE', #4105, .T. ) ;
#4326 = VECTOR ( 'NONE', #3589, 1000.000000000000000 ) ;
#4327 = EDGE_LOOP ( 'NONE', ( #3968, #3143, #2390, #3034, #2966, #2902, #2675, #371, #3298, #2382, #4917, #2874 ) ) ;
#4328 = VECTOR ( 'NONE', #2452, 1000.000000000000000 ) ;
#4329 = VECTOR ( 'NONE', #4665, 1000.000000000000000 ) ;
#4330 = CARTESIAN_POINT ( 'NONE',  ( 2.500000000000000000, 1.178949249685213863, -2.042000000000001148 ) ) ;
#4331 = VECTOR ( 'NONE', #1578, 1000.000000000000000 ) ;
#4332 = CIRCLE ( 'NONE', #817, 1.610000000000000098 ) ;
#4333 = LINE ( 'NONE', #3961, #3155 ) ;
#4334 = ORIENTED_EDGE ( 'NONE', *, *, #196, .F. ) ;
#4335 = ORIENTED_EDGE ( 'NONE', *, *, #1478, .T. ) ;
#4336 = VECTOR ( 'NONE', #3249, 1000.000000000000114 ) ;
#4337 =( GEOMETRIC_REPRESENTATION_CONTEXT ( 3 ) GLOBAL_UNCERTAINTY_ASSIGNED_CONTEXT ( ( #1490 ) ) GLOBAL_UNIT_ASSIGNED_CONTEXT ( ( #4932, #347, #2648 ) ) REPRESENTATION_CONTEXT ( 'NONE', 'WORKASPACE' ) );
#4338 = DIRECTION ( 'NONE',  ( 0.000000000000000000, 0.4999999999999990008, -0.8660254037844391517 ) ) ;
#4339 = ADVANCED_FACE ( 'NONE', ( #3265 ), #3656, .T. ) ;
#4340 = DIRECTION ( 'NONE',  ( 0.000000000000000000, 0.000000000000000000, -1.000000000000000000 ) ) ;
#4341 = AXIS2_PLACEMENT_3D ( 'NONE', #3115, #1207, #3215 ) ;
#4342 = LINE ( 'NONE', #1711, #1533 ) ;
#4343 = PRESENTATION_LAYER_ASSIGNMENT (  '', '', ( #1538 ) ) ;
#4344 = ORIENTED_EDGE ( 'NONE', *, *, #4424, .F. ) ;
#4345 = AXIS2_PLACEMENT_3D ( 'NONE', #302, #2833, #2099 ) ;
#4346 = VERTEX_POINT ( 'NONE', #4889 ) ;
#4347 = CARTESIAN_POINT ( 'NONE',  ( 0.000000000000000000, 2.357898499370433054, -1.951563910473907981E-15 ) ) ;
#4348 = CARTESIAN_POINT ( 'NONE',  ( 0.000000000000000000, -25.00000000000000000, -32.00000000000000000 ) ) ;
#4349 = CARTESIAN_POINT ( 'NONE',  ( 6.497531322021036645E-14, -16.00000000000000000, -26.00000000000000355 ) ) ;
#4350 = AXIS2_PLACEMENT_3D ( 'NONE', #662, #2196, #3719 ) ;
#4351 = VERTEX_POINT ( 'NONE', #605 ) ;
#4352 = CARTESIAN_POINT ( 'NONE',  ( 0.000000000000000000, 25.00000000000000000, -32.00000000000000000 ) ) ;
#4353 = CARTESIAN_POINT ( 'NONE',  ( -25.00000000000000000, 3.061616997868383043E-15, -1.999999999999994893 ) ) ;
#4354 = EDGE_LOOP ( 'NONE', ( #1218, #1422, #90, #1014, #3405, #36 ) ) ;
#4355 = AXIS2_PLACEMENT_3D ( 'NONE', #4147, #1548, #767 ) ;
#4356 = EDGE_CURVE ( 'NONE', #3611, #3321, #1057, .T. ) ;
#4357 = CARTESIAN_POINT ( 'NONE',  ( -3.642919299551294898E-14, -16.00000000000000000, -28.64999999999999858 ) ) ;
#4358 = CARTESIAN_POINT ( 'NONE',  ( -7.332110811570578784E-14, -6.999999999999999112, -32.00000000000000000 ) ) ;
#4359 = VERTEX_POINT ( 'NONE', #4452 ) ;
#4360 = ORIENTED_EDGE ( 'NONE', *, *, #1935, .F. ) ;
#4361 = PRODUCT_DEFINITION ( 'UNKNOWN', '', #2551, #2734 ) ;
#4362 = ADVANCED_FACE ( 'NONE', ( #1082 ), #1029, .T. ) ;
#4363 = CARTESIAN_POINT ( 'NONE',  ( 0.000000000000000000, 0.000000000000000000, -4.000000000000000000 ) ) ;
#4364 = CARTESIAN_POINT ( 'NONE',  ( 0.000000000000000000, 0.000000000000000000, -12.00000000000000000 ) ) ;
#4365 = DIRECTION ( 'NONE',  ( -0.000000000000000000, -0.000000000000000000, 1.000000000000000000 ) ) ;
#4366 = ORIENTED_EDGE ( 'NONE', *, *, #2400, .T. ) ;
#4367 = EDGE_CURVE ( 'NONE', #3754, #2727, #1524, .T. ) ;
#4368 = ORIENTED_EDGE ( 'NONE', *, *, #963, .F. ) ;
#4369 = CARTESIAN_POINT ( 'NONE',  ( 0.000000000000000000, 0.000000000000000000, 12.00000000000000000 ) ) ;
#4370 = CARTESIAN_POINT ( 'NONE',  ( -25.00000000000000000, 3.061616997868383043E-15, -20.00000000000000000 ) ) ;
#4371 = DIRECTION ( 'NONE',  ( 1.000000000000000000, 0.000000000000000000, 0.000000000000000000 ) ) ;
#4372 = VERTEX_POINT ( 'NONE', #3070 ) ;
#4373 = DIRECTION ( 'NONE',  ( 0.000000000000000000, 0.000000000000000000, -1.000000000000000000 ) ) ;
#4374 = CARTESIAN_POINT ( 'NONE',  ( 0.000000000000000000, 0.000000000000000000, -4.000000000000000000 ) ) ;
#4375 = CARTESIAN_POINT ( 'NONE',  ( 21.87894646962818612, -12.09631101282777266, -31.22510989603295428 ) ) ;
#4376 = ORIENTED_EDGE ( 'NONE', *, *, #3186, .F. ) ;
#4377 = DIRECTION ( 'NONE',  ( -1.000000000000000000, 0.000000000000000000, 0.000000000000000000 ) ) ;
#4378 = APPLICATION_PROTOCOL_DEFINITION ( 'draft international standard', 'automotive_design', 1998, #4442 ) ;
#4379 = SURFACE_STYLE_FILL_AREA ( #3960 ) ;
#4380 = ADVANCED_FACE ( 'NONE', ( #725 ), #1856, .F. ) ;
#4381 = STYLED_ITEM ( 'NONE', ( #452 ), #345 ) ;
#4382 = ORIENTED_EDGE ( 'NONE', *, *, #4160, .F. ) ;
#4383 = CARTESIAN_POINT ( 'NONE',  ( -23.68543856465402797, 7.999999999999996447, -4.000000000000000000 ) ) ;
#4384 = PLANE ( 'NONE',  #1052 ) ;
#4385 = CARTESIAN_POINT ( 'NONE',  ( -23.68543856465402442, -8.000000000000003553, -12.00000000000000000 ) ) ;
#4386 = ORIENTED_EDGE ( 'NONE', *, *, #623, .T. ) ;
#4387 = ORIENTED_EDGE ( 'NONE', *, *, #4173, .T. ) ;
#4388 = CARTESIAN_POINT ( 'NONE',  ( 2.000000000000000000, -0.8865213383406690406, 1.535500000000000975 ) ) ;
#4389 = DIRECTION ( 'NONE',  ( -1.000000000000000000, 0.000000000000000000, 0.000000000000000000 ) ) ;
#4390 = EDGE_CURVE ( 'NONE', #3704, #2143, #1185, .T. ) ;
#4391 = ADVANCED_FACE ( 'NONE', ( #2712 ), #2691, .F. ) ;
#4392 = ORIENTED_EDGE ( 'NONE', *, *, #3653, .T. ) ;
#4393 = LINE ( 'NONE', #531, #1351 ) ;
#4394 = CARTESIAN_POINT ( 'NONE',  ( 21.86452818504794138, -12.12206676558875529, -31.00832769771325559 ) ) ;
#4395 = VERTEX_POINT ( 'NONE', #4553 ) ;
#4396 = VECTOR ( 'NONE', #3481, 1000.000000000000000 ) ;
#4397 = DIRECTION ( 'NONE',  ( -1.000000000000000000, 0.000000000000000000, -0.000000000000000000 ) ) ;
#4398 = SURFACE_STYLE_USAGE ( .BOTH. , #856 ) ;
#4399 = VECTOR ( 'NONE', #3549, 1000.000000000000000 ) ;
#4400 = ORIENTED_EDGE ( 'NONE', *, *, #2845, .F. ) ;
#4401 = ADVANCED_FACE ( 'NONE', ( #3005 ), #4916, .T. ) ;
#4402 = CIRCLE ( 'NONE', #1442, 2.055000000000000160 ) ;
#4403 = DIRECTION ( 'NONE',  ( -0.000000000000000000, -0.000000000000000000, 1.000000000000000000 ) ) ;
#4404 = DIRECTION ( 'NONE',  ( -0.000000000000000000, -0.000000000000000000, 1.000000000000000000 ) ) ;
#4405 = CARTESIAN_POINT ( 'NONE',  ( -9.000000000000001776, 3.903127820947817540E-15, -12.00000000000000000 ) ) ;
#4406 = VECTOR ( 'NONE', #52, 1000.000000000000000 ) ;
#4407 = CONICAL_SURFACE ( 'NONE', #896, 1.535500000000000087, 1.047197551196590748 ) ;
#4408 = ORIENTED_EDGE ( 'NONE', *, *, #2140, .F. ) ;
#4409 = EDGE_CURVE ( 'NONE', #1320, #2431, #2665, .T. ) ;
#4410 = VERTEX_POINT ( 'NONE', #3095 ) ;
#4411 = EDGE_CURVE ( 'NONE', #1819, #1050, #2304, .T. ) ;
#4412 = AXIS2_PLACEMENT_3D ( 'NONE', #2570, #2623, #2645 ) ;
#4413 = CARTESIAN_POINT ( 'NONE',  ( 6.517431832507181422E-14, -16.00000000000000000, -23.90000000000000568 ) ) ;
#4414 = CYLINDRICAL_SURFACE ( 'NONE', #892, 2.649999999999992806 ) ;
#4415 = DIRECTION ( 'NONE',  ( -1.000000000000000000, 3.578554360455198522E-15, 0.000000000000000000 ) ) ;
#4416 = ORIENTED_EDGE ( 'NONE', *, *, #172, .T. ) ;
#4417 = CIRCLE ( 'NONE', #4662, 1.535500000000000087 ) ;
#4418 = CARTESIAN_POINT ( 'NONE',  ( 8.500000000000000000, -21.37171027316251681, 4.000000000000000000 ) ) ;
#4419 = EDGE_CURVE ( 'NONE', #3852, #571, #404, .T. ) ;
#4420 = DIRECTION ( 'NONE',  ( 0.000000000000000000, 0.000000000000000000, -1.000000000000000000 ) ) ;
#4421 = CARTESIAN_POINT ( 'NONE',  ( 0.000000000000000000, -0.8865213383406690406, 1.535500000000000975 ) ) ;
#4422 = AXIS2_PLACEMENT_3D ( 'NONE', #944, #3641, #1359 ) ;
#4423 = EDGE_LOOP ( 'NONE', ( #760, #3663, #456, #1751 ) ) ;
#4424 = EDGE_CURVE ( 'NONE', #1319, #4892, #1557, .T. ) ;
#4425 = CARTESIAN_POINT ( 'NONE',  ( 0.000000000000000000, 0.000000000000000000, -4.000000000000000000 ) ) ;
#4426 = PLANE ( 'NONE',  #1058 ) ;
#4427 = CIRCLE ( 'NONE', #594, 25.00000000000000000 ) ;
#4428 = ORIENTED_EDGE ( 'NONE', *, *, #2952, .F. ) ;
#4429 = AXIS2_PLACEMENT_3D ( 'NONE', #3530, #2060, #4682 ) ;
#4430 = DIRECTION ( 'NONE',  ( -1.000000000000000000, -0.000000000000000000, -0.000000000000000000 ) ) ;
#4431 = CARTESIAN_POINT ( 'NONE',  ( 0.000000000000000000, 0.000000000000000000, 12.00000000000000000 ) ) ;
#4432 = ORIENTED_EDGE ( 'NONE', *, *, #1976, .F. ) ;
#4433 = DIRECTION ( 'NONE',  ( 0.000000000000000000, 0.000000000000000000, -1.000000000000000000 ) ) ;
#4434 = CARTESIAN_POINT ( 'NONE',  ( 2.000000000000000000, -0.8865213383406721492, -1.535499999999999199 ) ) ;
#4435 = DIRECTION ( 'NONE',  ( -1.106769389831504682E-16, -1.000000000000000000, 0.000000000000000000 ) ) ;
#4436 = CARTESIAN_POINT ( 'NONE',  ( 0.000000000000000000, 0.000000000000000000, -4.000000000000000000 ) ) ;
#4437 = EDGE_CURVE ( 'NONE', #1327, #4023, #4225, .T. ) ;
#4438 = ORIENTED_EDGE ( 'NONE', *, *, #2898, .T. ) ;
#4439 = DIRECTION ( 'NONE',  ( 0.000000000000000000, 0.000000000000000000, -1.000000000000000000 ) ) ;
#4440 = CARTESIAN_POINT ( 'NONE',  ( 22.03949535914419400, 11.80087472665740655, -21.71428571428571885 ) ) ;
#4441 = FACE_OUTER_BOUND ( 'NONE', #22, .T. ) ;
#4442 = APPLICATION_CONTEXT ( 'automotive_design' ) ;
#4443 = VERTEX_POINT ( 'NONE', #3388 ) ;
#4444 = ADVANCED_FACE ( 'NONE', ( #2336 ), #3861, .T. ) ;
#4445 = PLANE ( 'NONE',  #2850 ) ;
#4446 = EDGE_CURVE ( 'NONE', #3165, #3494, #3018, .T. ) ;
#4447 = ADVANCED_FACE ( 'NONE', ( #1104 ), #1881, .T. ) ;
#4448 = ORIENTED_EDGE ( 'NONE', *, *, #3267, .T. ) ;
#4449 = CARTESIAN_POINT ( 'NONE',  ( 22.03949535914419400, 11.80087472665740655, -21.71428571428571885 ) ) ;
#4450 =( GEOMETRIC_REPRESENTATION_CONTEXT ( 3 ) GLOBAL_UNCERTAINTY_ASSIGNED_CONTEXT ( ( #790 ) ) GLOBAL_UNIT_ASSIGNED_CONTEXT ( ( #921, #544, #474 ) ) REPRESENTATION_CONTEXT ( 'NONE', 'WORKASPACE' ) );
#4451 = LINE ( 'NONE', #4863, #4810 ) ;
#4452 = CARTESIAN_POINT ( 'NONE',  ( 15.00000000000000000, 11.10102051443364068, -32.00000000000000000 ) ) ;
#4453 = ORIENTED_EDGE ( 'NONE', *, *, #2509, .F. ) ;
#4454 =( GEOMETRIC_REPRESENTATION_CONTEXT ( 3 ) GLOBAL_UNCERTAINTY_ASSIGNED_CONTEXT ( ( #1876 ) ) GLOBAL_UNIT_ASSIGNED_CONTEXT ( ( #4184, #3022, #2311 ) ) REPRESENTATION_CONTEXT ( 'NONE', 'WORKASPACE' ) );
#4455 = FACE_OUTER_BOUND ( 'NONE', #4544, .T. ) ;
#4456 = FILL_AREA_STYLE_COLOUR ( '', #3981 ) ;
#4457 = CARTESIAN_POINT ( 'NONE',  ( 15.00000000000000178, 16.00000000000000000, -26.00000000000000355 ) ) ;
#4458 = CARTESIAN_POINT ( 'NONE',  ( 21.97031423931356287, 11.92955703141275237, -20.40434499790757172 ) ) ;
#4459 = VERTEX_POINT ( 'NONE', #2549 ) ;
#4460 = DIRECTION ( 'NONE',  ( -1.000000000000000000, -0.000000000000000000, -0.000000000000000000 ) ) ;
#4461 = ORIENTED_EDGE ( 'NONE', *, *, #1361, .T. ) ;
#4462 = VERTEX_POINT ( 'NONE', #1397 ) ;
#4463 = PRODUCT_DEFINITION_FORMATION_WITH_SPECIFIED_SOURCE ( 'ANY', '', #613, .NOT_KNOWN. ) ;
#4464 = CARTESIAN_POINT ( 'NONE',  ( 5.200000000000002842, 0.000000000000000000, 2.500000000000000888 ) ) ;
#4465 = DIRECTION ( 'NONE',  ( 0.000000000000000000, 0.000000000000000000, -1.000000000000000000 ) ) ;
#4466 = DIRECTION ( 'NONE',  ( -1.000000000000000000, 0.000000000000000000, 0.000000000000000000 ) ) ;
#4467 = AXIS2_PLACEMENT_3D ( 'NONE', #4755, #2433, #3954 ) ;
#4468 = ORIENTED_EDGE ( 'NONE', *, *, #4481, .F. ) ;
#4469 = DIRECTION ( 'NONE',  ( -0.000000000000000000, -0.000000000000000000, 1.000000000000000000 ) ) ;
#4470 = VECTOR ( 'NONE', #1413, 1000.000000000000000 ) ;
#4471 = CARTESIAN_POINT ( 'NONE',  ( 0.000000000000000000, 0.8865213383406685965, -1.535500000000000753 ) ) ;
#4472 = ORIENTED_EDGE ( 'NONE', *, *, #2473, .F. ) ;
#4473 = VECTOR ( 'NONE', #1624, 1000.000000000000000 ) ;
#4474 = EDGE_CURVE ( 'NONE', #398, #3401, #248, .T. ) ;
#4475 = DIRECTION ( 'NONE',  ( -1.000000000000000000, 0.000000000000000000, 0.000000000000000000 ) ) ;
#4476 = AXIS2_PLACEMENT_3D ( 'NONE', #2223, #1465, #1818 ) ;
#4477 = DIRECTION ( 'NONE',  ( 0.000000000000000000, 0.000000000000000000, -1.000000000000000000 ) ) ;
#4478 = CARTESIAN_POINT ( 'NONE',  ( -14.00000000000006395, 16.00000000000000000, -26.00000000000000355 ) ) ;
#4479 = VERTEX_POINT ( 'NONE', #4857 ) ;
#4480 = VECTOR ( 'NONE', #610, 1000.000000000000000 ) ;
#4481 = EDGE_CURVE ( 'NONE', #4842, #4739, #2931, .T. ) ;
#4482 = PLANE ( 'NONE',  #118 ) ;
#4483 = CARTESIAN_POINT ( 'NONE',  ( 15.00000000000000178, -16.00000000000000000, -28.64999999999998792 ) ) ;
#4484 = AXIS2_PLACEMENT_3D ( 'NONE', #2487, #2119, #3633 ) ;
#4485 = DIRECTION ( 'NONE',  ( -0.000000000000000000, -0.000000000000000000, 1.000000000000000000 ) ) ;
#4486 = ORIENTED_EDGE ( 'NONE', *, *, #2278, .T. ) ;
#4487 = CONICAL_SURFACE ( 'NONE', #4171, 2.099999999999997868, 1.029744258676654090 ) ;
#4488 = AXIS2_PLACEMENT_3D ( 'NONE', #3794, #1172, #3084 ) ;
#4489 = CARTESIAN_POINT ( 'NONE',  ( 2.000000000000000000, -0.8865213383406690406, 1.535500000000000975 ) ) ;
#4490 = CARTESIAN_POINT ( 'NONE',  ( 22.03949535914419755, 11.80087472665740300, -30.28571428571428470 ) ) ;
#4491 = DIRECTION ( 'NONE',  ( -0.000000000000000000, 1.467581828789149729E-15, 1.000000000000000000 ) ) ;
#4492 = COLOUR_RGB ( '', 0.08235294, 0.09019608, 0.10196078) ;
#4493 = ORIENTED_EDGE ( 'NONE', *, *, #3119, .T. ) ;
#4494 = DIRECTION ( 'NONE',  ( -0.000000000000000000, -0.000000000000000000, 1.000000000000000000 ) ) ;
#4495 = PLANE ( 'NONE',  #1874 ) ;
#4496 = CONTEXT_DEPENDENT_SHAPE_REPRESENTATION ( #2306, #46 ) ;
#4497 = CARTESIAN_POINT ( 'NONE',  ( -3.666055405785289392E-14, -6.999999999999999112, -32.00000000000000000 ) ) ;
#4498 = EDGE_LOOP ( 'NONE', ( #1247, #4302, #2210, #2544 ) ) ;
#4499 = EDGE_CURVE ( 'NONE', #1024, #2366, #1370, .T. ) ;
#4500 = DIRECTION ( 'NONE',  ( -1.000000000000000000, 3.578554360455198522E-15, 0.000000000000000000 ) ) ;
#4501 = CARTESIAN_POINT ( 'NONE',  ( -4.473192950568998942E-14, -12.50000000000000178, -12.00000000000000000 ) ) ;
#4502 = CARTESIAN_POINT ( 'NONE',  ( 2.500000000000000000, -2.357898499370432610, 3.252606517456513302E-15 ) ) ;
#4503 = DIRECTION ( 'NONE',  ( 1.000000000000000000, 0.000000000000000000, 0.000000000000000000 ) ) ;
#4504 = ORIENTED_EDGE ( 'NONE', *, *, #776, .F. ) ;
#4505 = EDGE_CURVE ( 'NONE', #2974, #4182, #1073, .T. ) ;
#4506 = AXIS2_PLACEMENT_3D ( 'NONE', #221, #599, #3600 ) ;
#4507 = ORIENTED_EDGE ( 'NONE', *, *, #898, .T. ) ;
#4508 = DIRECTION ( 'NONE',  ( 1.000000000000000000, 0.000000000000000000, 0.000000000000000000 ) ) ;
#4509 = CARTESIAN_POINT ( 'NONE',  ( 25.00000000000000000, 0.000000000000000000, -4.000000000000000000 ) ) ;
#4510 = CARTESIAN_POINT ( 'NONE',  ( 0.000000000000000000, 25.00000000000000000, -20.00000000000000000 ) ) ;
#4511 = DIRECTION ( 'NONE',  ( 0.000000000000000000, -9.783878858594330870E-16, -1.000000000000000000 ) ) ;
#4512 = ADVANCED_FACE ( 'NONE', ( #2207 ), #1801, .T. ) ;
#4513 = ORIENTED_EDGE ( 'NONE', *, *, #548, .F. ) ;
#4514 = CARTESIAN_POINT ( 'NONE',  ( 15.00000000000000000, -11.10102051443364068, -31.00000000000000000 ) ) ;
#4515 = DIRECTION ( 'NONE',  ( -1.000000000000000000, 0.000000000000000000, 0.000000000000000000 ) ) ;
#4516 = CARTESIAN_POINT ( 'NONE',  ( -17.00000000000000000, 0.000000000000000000, -12.00000000000000000 ) ) ;
#4517 = ORIENTED_EDGE ( 'NONE', *, *, #2930, .F. ) ;
#4518 = DIRECTION ( 'NONE',  ( 1.000000000000000000, -0.000000000000000000, -0.000000000000000000 ) ) ;
#4519 = CARTESIAN_POINT ( 'NONE',  ( 0.000000000000000000, 0.000000000000000000, -20.00000000000000000 ) ) ;
#4520 = CONTEXT_DEPENDENT_SHAPE_REPRESENTATION ( #4537, #1838 ) ;
#4521 = DIRECTION ( 'NONE',  ( -1.000000000000000000, 0.000000000000000000, 0.000000000000000000 ) ) ;
#4522 = ORIENTED_EDGE ( 'NONE', *, *, #4609, .T. ) ;
#4523 = EDGE_CURVE ( 'NONE', #2491, #1504, #1822, .T. ) ;
#4524 = CARTESIAN_POINT ( 'NONE',  ( 0.000000000000000000, 25.00000000000000000, -32.00000000000000000 ) ) ;
#4525 = DIRECTION ( 'NONE',  ( -1.000000000000000000, 3.578554360455198522E-15, 0.000000000000000000 ) ) ;
#4526 = CARTESIAN_POINT ( 'NONE',  ( 2.000000000000000000, 1.773042676681340968, -2.276824562219559311E-15 ) ) ;
#4527 = CARTESIAN_POINT ( 'NONE',  ( 15.00000000000000000, -16.00000000000000000, -32.00000000000000000 ) ) ;
#4528 = ORIENTED_EDGE ( 'NONE', *, *, #2845, .T. ) ;
#4529 = DIRECTION ( 'NONE',  ( 1.000000000000000000, 0.000000000000000000, 0.000000000000000000 ) ) ;
#4530 = DIRECTION ( 'NONE',  ( 0.000000000000000000, 0.000000000000000000, 1.000000000000000000 ) ) ;
#4531 = LINE ( 'NONE', #4948, #2423 ) ;
#4532 = CARTESIAN_POINT ( 'NONE',  ( 12.49999999999999822, -19.30673457630782863, 12.00000000000000000 ) ) ;
#4533 = EDGE_CURVE ( 'NONE', #1467, #4937, #2081, .T. ) ;
#4534 = PLANE ( 'NONE',  #2593 ) ;
#4535 = ORIENTED_EDGE ( 'NONE', *, *, #400, .F. ) ;
#4536 = ORIENTED_EDGE ( 'NONE', *, *, #4409, .T. ) ;
#4537 =( REPRESENTATION_RELATIONSHIP ('NONE','NONE', #137, #1326 ) REPRESENTATION_RELATIONSHIP_WITH_TRANSFORMATION ( #1439 )SHAPE_REPRESENTATION_RELATIONSHIP( ) );
#4538 = DIRECTION ( 'NONE',  ( 1.000000000000000000, 0.000000000000000000, 0.000000000000000000 ) ) ;
#4539 =( LENGTH_UNIT ( ) NAMED_UNIT ( * ) SI_UNIT ( .MILLI., .METRE. ) );
#4540 = ADVANCED_FACE ( 'NONE', ( #4047 ), #319, .T. ) ;
#4541 = DIRECTION ( 'NONE',  ( -1.000000000000000000, 0.000000000000000000, 0.000000000000000000 ) ) ;
#4542 = ADVANCED_FACE ( 'NONE', ( #3330 ), #3308, .F. ) ;
#4543 = DIRECTION ( 'NONE',  ( -1.000000000000000000, 0.000000000000000000, 0.000000000000000000 ) ) ;
#4544 = EDGE_LOOP ( 'NONE', ( #4438, #4686, #3452 ) ) ;
#4545 = UNCERTAINTY_MEASURE_WITH_UNIT (LENGTH_MEASURE( 1.000000000000000082E-05 ), #976, 'distance_accuracy_value', 'NONE');
#4546 = DIRECTION ( 'NONE',  ( 1.106769389831504682E-16, 1.000000000000000000, 0.000000000000000000 ) ) ;
#4547 = EDGE_CURVE ( 'NONE', #3401, #4802, #3350, .T. ) ;
#4548 = ORIENTED_EDGE ( 'NONE', *, *, #4174, .T. ) ;
#4549 = VECTOR ( 'NONE', #3500, 1000.000000000000000 ) ;
#4550 = FACE_OUTER_BOUND ( 'NONE', #2063, .T. ) ;
#4551 = CYLINDRICAL_SURFACE ( 'NONE', #1537, 22.99999999999998934 ) ;
#4552 = DIRECTION ( 'NONE',  ( 0.000000000000000000, 0.000000000000000000, -1.000000000000000000 ) ) ;
#4553 = CARTESIAN_POINT ( 'NONE',  ( -6.708203932499367639, 2.000000000000000888, -12.00000000000000000 ) ) ;
#4554 = AXIS2_PLACEMENT_3D ( 'NONE', #1796, #3327, #1018 ) ;
#4555 = ORIENTED_EDGE ( 'NONE', *, *, #4437, .F. ) ;
#4556 = CONICAL_SURFACE ( 'NONE', #2247, 23.00000000000000711, 0.7853981633974473908 ) ;
#4557 = DIRECTION ( 'NONE',  ( 0.000000000000000000, 0.000000000000000000, 1.000000000000000000 ) ) ;
#4558 = CARTESIAN_POINT ( 'NONE',  ( 0.000000000000000000, 0.000000000000000000, -32.00000000000000000 ) ) ;
#4559 = FACE_OUTER_BOUND ( 'NONE', #1404, .T. ) ;
#4560 = DIRECTION ( 'NONE',  ( 1.000000000000000000, 0.000000000000000000, 0.000000000000000000 ) ) ;
#4561 = VECTOR ( 'NONE', #2123, 1000.000000000000000 ) ;
#4562 = ORIENTED_EDGE ( 'NONE', *, *, #4030, .F. ) ;
#4563 = EDGE_CURVE ( 'NONE', #165, #1875, #2720, .T. ) ;
#4564 = DIRECTION ( 'NONE',  ( 1.000000000000000000, 0.000000000000000000, 0.000000000000000000 ) ) ;
#4565 = CIRCLE ( 'NONE', #256, 2.000000000000000888 ) ;
#4566 = CARTESIAN_POINT ( 'NONE',  ( -12.50000000000000178, 19.30673457630782863, 12.00000000000000000 ) ) ;
#4567 = AXIS2_PLACEMENT_3D ( 'NONE', #3888, #4231, #861 ) ;
#4568 = VERTEX_POINT ( 'NONE', #4123 ) ;
#4569 = VECTOR ( 'NONE', #199, 1000.000000000000000 ) ;
#4570 = CIRCLE ( 'NONE', #2262, 2.649999999999995914 ) ;
#4571 = VECTOR ( 'NONE', #2886, 1000.000000000000000 ) ;
#4572 = EDGE_CURVE ( 'NONE', #2953, #2498, #3666, .T. ) ;
#4573 = CYLINDRICAL_SURFACE ( 'NONE', #713, 17.00000000000000000 ) ;
#4574 = CARTESIAN_POINT ( 'NONE',  ( -4.336808689942023652E-16, 2.000000000000002220, -20.00000000000000000 ) ) ;
#4575 = AXIS2_PLACEMENT_3D ( 'NONE', #753, #2634, #3432 ) ;
#4576 = MECHANICAL_DESIGN_GEOMETRIC_PRESENTATION_REPRESENTATION (  '', ( #1538 ), #823 ) ;
#4577 = ORIENTED_EDGE ( 'NONE', *, *, #708, .T. ) ;
#4578 = EDGE_LOOP ( 'NONE', ( #4709, #3786, #2518, #1261 ) ) ;
#4579 = EDGE_CURVE ( 'NONE', #4003, #4613, #1843, .T. ) ;
#4580 = EDGE_CURVE ( 'NONE', #467, #4063, #1046, .T. ) ;
#4581 = CLOSED_SHELL ( 'NONE', ( #3990, #483, #4391, #1178, #4722, #3304, #2533, #4634, #1329, #4069, #1421, #3878, #2358, #4196, #4362, #4856, #4540, #2012, #4401, #3478, #4146, #3658, #1853, #3484, #3467, #4305, #2465, #2225, #2132 ) ) ;
#4582 = AXIS2_PLACEMENT_3D ( 'NONE', #2759, #3353, #3875 ) ;
#4583 = CARTESIAN_POINT ( 'NONE',  ( 22.82279522939548144, -10.20431389251127285, -24.39513802366778705 ) ) ;
#4584 = DIRECTION ( 'NONE',  ( -1.000000000000000000, 0.000000000000000000, -0.000000000000000000 ) ) ;
#4585 = FACE_OUTER_BOUND ( 'NONE', #2880, .T. ) ;
#4586 = VECTOR ( 'NONE', #4415, 1000.000000000000000 ) ;
#4587 = CARTESIAN_POINT ( 'NONE',  ( 0.000000000000000000, 0.000000000000000000, -4.000000000000000000 ) ) ;
#4588 = ORIENTED_EDGE ( 'NONE', *, *, #3186, .T. ) ;
#4589 = AXIS2_PLACEMENT_3D ( 'NONE', #4706, #1628, #1652 ) ;
#4590 = CARTESIAN_POINT ( 'NONE',  ( 0.000000000000000000, 0.000000000000000000, 0.000000000000000000 ) ) ;
#4591 = CARTESIAN_POINT ( 'NONE',  ( -15.57269238203818063, 20.33448430559305109, 25.99999999999999645 ) ) ;
#4592 = CARTESIAN_POINT ( 'NONE',  ( 23.68543856465402442, -8.000000000000003553, -12.00000000000000000 ) ) ;
#4593 = DIRECTION ( 'NONE',  ( -1.000000000000000000, 0.000000000000000000, 0.000000000000000000 ) ) ;
#4594 = CARTESIAN_POINT ( 'NONE',  ( 22.30769810302473033, -11.28612666381333440, -20.01290653110665119 ) ) ;
#4595 = AXIS2_PLACEMENT_3D ( 'NONE', #3280, #2579, #1419 ) ;
#4596 = ORIENTED_EDGE ( 'NONE', *, *, #3475, .T. ) ;
#4597 = ORIENTED_EDGE ( 'NONE', *, *, #3941, .F. ) ;
#4598 = CARTESIAN_POINT ( 'NONE',  ( 0.000000000000000000, -25.00000000000000000, -32.00000000000000000 ) ) ;
#4599 = FILL_AREA_STYLE_COLOUR ( '', #1454 ) ;
#4600 = EDGE_CURVE ( 'NONE', #1395, #115, #1097, .T. ) ;
#4601 = EDGE_LOOP ( 'NONE', ( #1489, #3937, #842 ) ) ;
#4602 = UNCERTAINTY_MEASURE_WITH_UNIT (LENGTH_MEASURE( 1.000000000000000082E-05 ), #3420, 'distance_accuracy_value', 'NONE');
#4603 =( NAMED_UNIT ( * ) SI_UNIT ( $, .STERADIAN. ) SOLID_ANGLE_UNIT ( ) );
#4604 = EDGE_CURVE ( 'NONE', #4073, #1313, #1505, .T. ) ;
#4605 = ORIENTED_EDGE ( 'NONE', *, *, #2816, .F. ) ;
#4606 = EDGE_CURVE ( 'NONE', #212, #2765, #458, .T. ) ;
#4607 = EDGE_LOOP ( 'NONE', ( #3537, #460, #1436, #2158, #3085, #4710 ) ) ;
#4608 = EDGE_CURVE ( 'NONE', #1339, #4175, #4314, .T. ) ;
#4609 = EDGE_CURVE ( 'NONE', #3747, #1716, #1280, .T. ) ;
#4610 = FACE_OUTER_BOUND ( 'NONE', #1639, .T. ) ;
#4611 = CARTESIAN_POINT ( 'NONE',  ( -6.708203932499366751, -2.000000000000003553, -20.00000000000000000 ) ) ;
#4612 =( REPRESENTATION_RELATIONSHIP ('NONE','NONE', #137, #2032 ) REPRESENTATION_RELATIONSHIP_WITH_TRANSFORMATION ( #837 )SHAPE_REPRESENTATION_RELATIONSHIP( ) );
#4613 = VERTEX_POINT ( 'NONE', #394 ) ;
#4614 = CARTESIAN_POINT ( 'NONE',  ( 0.000000000000000000, 0.000000000000000000, 0.000000000000000000 ) ) ;
#4615 = DIRECTION ( 'NONE',  ( -0.000000000000000000, -0.000000000000000000, -1.000000000000000000 ) ) ;
#4616 = DIRECTION ( 'NONE',  ( 0.000000000000000000, -1.000000000000000000, 0.000000000000000000 ) ) ;
#4617 = CARTESIAN_POINT ( 'NONE',  ( 21.88691174701116537, 12.08152700620044939, -31.22242340959439133 ) ) ;
#4618 = VERTEX_POINT ( 'NONE', #1872 ) ;
#4619 = EDGE_LOOP ( 'NONE', ( #3427, #1332, #4203, #3561 ) ) ;
#4620 = FILL_AREA_STYLE_COLOUR ( '', #3737 ) ;
#4621 = FACE_OUTER_BOUND ( 'NONE', #1346, .T. ) ;
#4622 = DIRECTION ( 'NONE',  ( -1.000000000000000000, 0.000000000000000000, 0.000000000000000000 ) ) ;
#4623 = DIRECTION ( 'NONE',  ( 0.5150380749100544886, 0.000000000000000000, -0.8571673007021121116 ) ) ;
#4624 = ORIENTED_EDGE ( 'NONE', *, *, #1758, .T. ) ;
#4625 = DIRECTION ( 'NONE',  ( -0.000000000000000000, -0.000000000000000000, 1.000000000000000000 ) ) ;
#4626 = DIRECTION ( 'NONE',  ( 1.000000000000000000, 0.000000000000000000, 0.000000000000000000 ) ) ;
#4627 = ORIENTED_EDGE ( 'NONE', *, *, #2620, .T. ) ;
#4628 = EDGE_LOOP ( 'NONE', ( #4248, #1125, #3568, #4877, #1932, #3102, #4461, #834, #744 ) ) ;
#4629 = PRODUCT_DEFINITION_CONTEXT ( 'detailed design', #1891, 'design' ) ;
#4630 = CARTESIAN_POINT ( 'NONE',  ( -10.00000000000002132, 16.00000000000000000, -26.00000000000000355 ) ) ;
#4631 = LINE ( 'NONE', #1184, #337 ) ;
#4632 = ORIENTED_EDGE ( 'NONE', *, *, #1415, .F. ) ;
#4633 = ORIENTED_EDGE ( 'NONE', *, *, #2253, .T. ) ;
#4634 = ADVANCED_FACE ( 'NONE', ( #2275 ), #1151, .T. ) ;
#4635 = MECHANICAL_DESIGN_GEOMETRIC_PRESENTATION_REPRESENTATION (  '', ( #4230 ), #1821 ) ;
#4636 = DIRECTION ( 'NONE',  ( -0.000000000000000000, -0.000000000000000000, 1.000000000000000000 ) ) ;
#4637 = CARTESIAN_POINT ( 'NONE',  ( 2.000000000000000000, 0.8865213383406685965, -1.535500000000000753 ) ) ;
#4638 = ORIENTED_EDGE ( 'NONE', *, *, #2852, .F. ) ;
#4639 = EDGE_CURVE ( 'NONE', #852, #54, #850, .T. ) ;
#4640 = AXIS2_PLACEMENT_3D ( 'NONE', #2547, #4853, #638 ) ;
#4641 = ORIENTED_EDGE ( 'NONE', *, *, #2760, .F. ) ;
#4642 =( NAMED_UNIT ( * ) PLANE_ANGLE_UNIT ( ) SI_UNIT ( $, .RADIAN. ) );
#4643 = FACE_OUTER_BOUND ( 'NONE', #3028, .T. ) ;
#4644 = DIRECTION ( 'NONE',  ( -1.000000000000000000, -4.073394895316987600E-15, 0.000000000000000000 ) ) ;
#4645 = CARTESIAN_POINT ( 'NONE',  ( 2.500000000000000000, -1.178949249685213863, 2.042000000000002924 ) ) ;
#4646 = AXIS2_PLACEMENT_3D ( 'NONE', #1147, #2678, #2294 ) ;
#4647 = ORIENTED_EDGE ( 'NONE', *, *, #3318, .F. ) ;
#4648 = VECTOR ( 'NONE', #4435, 1000.000000000000000 ) ;
#4649 = AXIS2_PLACEMENT_3D ( 'NONE', #2745, #4615, #4285 ) ;
#4650 = CARTESIAN_POINT ( 'NONE',  ( -14.00000000000006395, 16.00000000000000000, -28.10000000000000142 ) ) ;
#4651 = CARTESIAN_POINT ( 'NONE',  ( -3.666055405785289392E-14, -6.999999999999999112, -20.00000000000000000 ) ) ;
#4652 = EDGE_LOOP ( 'NONE', ( #3124, #3729, #1994 ) ) ;
#4653 = AXIS2_PLACEMENT_3D ( 'NONE', #4108, #4552, #752 ) ;
#4654 = VECTOR ( 'NONE', #4338, 1000.000000000000227 ) ;
#4655 = VERTEX_POINT ( 'NONE', #4934 ) ;
#4656 = AXIS2_PLACEMENT_3D ( 'NONE', #4223, #3037, #1159 ) ;
#4657 = CARTESIAN_POINT ( 'NONE',  ( 22.87713223651540417, -10.08160808888848514, -24.99301090304139095 ) ) ;
#4658 = CARTESIAN_POINT ( 'NONE',  ( -3.666055405785289392E-14, -6.999999999999999112, -32.00000000000000000 ) ) ;
#4659 = DIRECTION ( 'NONE',  ( -1.000000000000000000, 0.000000000000000000, 0.000000000000000000 ) ) ;
#4660 = EDGE_CURVE ( 'NONE', #3700, #987, #2554, .T. ) ;
#4661 = ORIENTED_EDGE ( 'NONE', *, *, #463, .F. ) ;
#4662 = AXIS2_PLACEMENT_3D ( 'NONE', #3139, #4683, #2387 ) ;
#4663 = ORIENTED_EDGE ( 'NONE', *, *, #4235, .F. ) ;
#4664 = APPLICATION_PROTOCOL_DEFINITION ( 'draft international standard', 'automotive_design', 1998, #768 ) ;
#4665 = DIRECTION ( 'NONE',  ( -0.000000000000000000, -0.000000000000000000, 1.000000000000000000 ) ) ;
#4666 = CARTESIAN_POINT ( 'NONE',  ( -3.642919299551294898E-14, -16.00000000000000000, -23.35000000000000497 ) ) ;
#4667 = PLANE ( 'NONE',  #2748 ) ;
#4668 = PRODUCT_RELATED_PRODUCT_CATEGORY ( 'part', '', ( #1374 ) ) ;
#4669 = EDGE_CURVE ( 'NONE', #941, #2762, #3880, .T. ) ;
#4670 = VERTEX_POINT ( 'NONE', #2682 ) ;
#4671 = EDGE_LOOP ( 'NONE', ( #1194, #3588 ) ) ;
#4672 = LINE ( 'NONE', #2757, #4161 ) ;
#4673 = DIRECTION ( 'NONE',  ( 0.000000000000000000, 0.000000000000000000, -1.000000000000000000 ) ) ;
#4674 = CARTESIAN_POINT ( 'NONE',  ( 2.172477277502393807E-14, -16.00000000000000000, -26.00000000000000355 ) ) ;
#4675 = EDGE_CURVE ( 'NONE', #1319, #2396, #3125, .T. ) ;
#4676 = EDGE_LOOP ( 'NONE', ( #2101, #1563, #3516, #1105 ) ) ;
#4677 = CIRCLE ( 'NONE', #2523, 23.00000000000000711 ) ;
#4678 = LINE ( 'NONE', #1324, #3593 ) ;
#4679 = CARTESIAN_POINT ( 'NONE',  ( 2.000000000000000000, 1.329782007511004727, -0.7677500000000019309 ) ) ;
#4680 = ORIENTED_EDGE ( 'NONE', *, *, #3295, .F. ) ;
#4681 = ORIENTED_EDGE ( 'NONE', *, *, #513, .T. ) ;
#4682 = DIRECTION ( 'NONE',  ( 0.000000000000000000, 0.000000000000000000, -1.000000000000000000 ) ) ;
#4683 = DIRECTION ( 'NONE',  ( -1.000000000000000000, -0.000000000000000000, -0.000000000000000000 ) ) ;
#4684 = CARTESIAN_POINT ( 'NONE',  ( 2.500000000000000000, 0.000000000000000000, 0.000000000000000000 ) ) ;
#4685 = VERTEX_POINT ( 'NONE', #1491 ) ;
#4686 = ORIENTED_EDGE ( 'NONE', *, *, #4356, .T. ) ;
#4687 = DIRECTION ( 'NONE',  ( 0.000000000000000000, 0.000000000000000000, -1.000000000000000000 ) ) ;
#4688 = PLANE ( 'NONE',  #3604 ) ;
#4689 = CARTESIAN_POINT ( 'NONE',  ( -12.50000000000000000, -1.383461737289380927E-15, 12.00000000000000000 ) ) ;
#4690 = VERTEX_POINT ( 'NONE', #3450 ) ;
#4691 = EDGE_LOOP ( 'NONE', ( #3630, #2144, #3324, #635, #2861, #1984, #4627, #1679 ) ) ;
#4692 = SHAPE_REPRESENTATION_RELATIONSHIP ( 'NONE' , 'NONE' ,  #2032, #345 ) ;
#4693 = CARTESIAN_POINT ( 'NONE',  ( 2.500000000000000000, 2.357898499370433054, -1.951563910473907981E-15 ) ) ;
#4694 = LINE ( 'NONE', #4348, #2507 ) ;
#4695 = ORIENTED_EDGE ( 'NONE', *, *, #1333, .T. ) ;
#4696 = ADVANCED_FACE ( 'NONE', ( #3033 ), #1175, .F. ) ;
#4697 = ADVANCED_FACE ( 'NONE', ( #1199 ), #4169, .T. ) ;
#4698 = EDGE_CURVE ( 'NONE', #216, #2709, #3480, .T. ) ;
#4699 = DIRECTION ( 'NONE',  ( -0.5000000000000051070, 1.060575238724903217E-16, -0.8660254037844355990 ) ) ;
#4700 = CARTESIAN_POINT ( 'NONE',  ( -8.500000000000003553, 21.37171027316251681, 4.000000000000000000 ) ) ;
#4701 = ORIENTED_EDGE ( 'NONE', *, *, #870, .T. ) ;
#4702 = ORIENTED_EDGE ( 'NONE', *, *, #1027, .T. ) ;
#4703 = AXIS2_PLACEMENT_3D ( 'NONE', #4591, #3758, #1165 ) ;
#4704 = EDGE_CURVE ( 'NONE', #45, #645, #1514, .T. ) ;
#4705 = EDGE_CURVE ( 'NONE', #3536, #865, #2654, .T. ) ;
#4706 = CARTESIAN_POINT ( 'NONE',  ( 15.00000000000000178, -16.00000000000000000, -26.00000000000000355 ) ) ;
#4707 =( LENGTH_UNIT ( ) NAMED_UNIT ( * ) SI_UNIT ( .MILLI., .METRE. ) );
#4708 = DIRECTION ( 'NONE',  ( -0.000000000000000000, 0.000000000000000000, 1.000000000000000000 ) ) ;
#4709 = ORIENTED_EDGE ( 'NONE', *, *, #1182, .F. ) ;
#4710 = ORIENTED_EDGE ( 'NONE', *, *, #1996, .F. ) ;
#4711 = PRODUCT_DEFINITION_FORMATION_WITH_SPECIFIED_SOURCE ( 'ANY', '', #853, .NOT_KNOWN. ) ;
#4712 = CARTESIAN_POINT ( 'NONE',  ( 15.00000000000000000, 11.80087472665740655, -21.71428571428571885 ) ) ;
#4713 = FACE_OUTER_BOUND ( 'NONE', #3282, .T. ) ;
#4714 = VECTOR ( 'NONE', #3278, 1000.000000000000000 ) ;
#4715 = CARTESIAN_POINT ( 'NONE',  ( -17.00000000000000000, 0.000000000000000000, -4.000000000000000000 ) ) ;
#4716 = VERTEX_POINT ( 'NONE', #4650 ) ;
#4717 = COLOUR_RGB ( '', 0.40784314, 0.44705882, 0.49803922) ;
#4718 = ORIENTED_EDGE ( 'NONE', *, *, #4737, .F. ) ;
#4719 = DIRECTION ( 'NONE',  ( -1.000000000000000000, -0.000000000000000000, -0.000000000000000000 ) ) ;
#4720 = CYLINDRICAL_SURFACE ( 'NONE', #1777, 4.250000000000000000 ) ;
#4721 = CARTESIAN_POINT ( 'NONE',  ( 22.40016391766193138, 11.10102051443364424, -20.00000000000000000 ) ) ;
#4722 = ADVANCED_FACE ( 'NONE', ( #1228 ), #4573, .F. ) ;
#4723 = CIRCLE ( 'NONE', #2563, 1.000000000000000888 ) ;
#4724 = EDGE_CURVE ( 'NONE', #1179, #3810, #2159, .T. ) ;
#4725 = ORIENTED_EDGE ( 'NONE', *, *, #11, .F. ) ;
#4726 = CARTESIAN_POINT ( 'NONE',  ( 19.20937271229854915, -11.10102051443364424, -20.00000000000000000 ) ) ;
#4727 = DIRECTION ( 'NONE',  ( -1.000000000000000000, 0.000000000000000000, 0.000000000000000000 ) ) ;
#4728 = VECTOR ( 'NONE', #1434, 1000.000000000000000 ) ;
#4729 = EDGE_CURVE ( 'NONE', #991, #1722, #396, .T. ) ;
#4730 = ORIENTED_EDGE ( 'NONE', *, *, #3907, .T. ) ;
#4731 = ADVANCED_FACE ( 'NONE', ( #3162 ), #1274, .T. ) ;
#4732 = AXIS2_PLACEMENT_3D ( 'NONE', #2393, #57, #3122 ) ;
#4733 = DIRECTION ( 'NONE',  ( -1.000000000000000000, -0.000000000000000000, -0.000000000000000000 ) ) ;
#4734 = CARTESIAN_POINT ( 'NONE',  ( 7.216449660063538023E-15, 2.136559688479409280E-14, -12.00000000000000000 ) ) ;
#4735 = AXIS2_PLACEMENT_3D ( 'NONE', #3984, #1349, #2445 ) ;
#4736 = CARTESIAN_POINT ( 'NONE',  ( 0.000000000000000000, 0.000000000000000000, 4.000000000000000000 ) ) ;
#4737 = EDGE_CURVE ( 'NONE', #4838, #3126, #3995, .T. ) ;
#4738 = VERTEX_POINT ( 'NONE', #927 ) ;
#4739 = VERTEX_POINT ( 'NONE', #2476 ) ;
#4740 = CIRCLE ( 'NONE', #3613, 1.000000000000000888 ) ;
#4741 = CIRCLE ( 'NONE', #3694, 23.00000000000000711 ) ;
#4742 = VECTOR ( 'NONE', #3272, 1000.000000000000000 ) ;
#4743 = CARTESIAN_POINT ( 'NONE',  ( -6.708203932499366751, -2.000000000000003553, -12.00000000000000000 ) ) ;
#4744 = VECTOR ( 'NONE', #1575, 1000.000000000000000 ) ;
#4745 = DIRECTION ( 'NONE',  ( -0.9474175425861609545, -0.3199999999999996181, 0.000000000000000000 ) ) ;
#4746 = VECTOR ( 'NONE', #1111, 1000.000000000000000 ) ;
#4747 = VERTEX_POINT ( 'NONE', #167 ) ;
#4748 = SHAPE_REPRESENTATION ( 'socket head cap screw_iso_ISO 4762 M5 x 20 - 20N', ( #1918 ), #3816 ) ;
#4749 = AXIS2_PLACEMENT_3D ( 'NONE', #4674, #1948, #3160 ) ;
#4750 = ORIENTED_EDGE ( 'NONE', *, *, #4174, .F. ) ;
#4751 = DIRECTION ( 'NONE',  ( -1.000000000000000000, -0.000000000000000000, -0.000000000000000000 ) ) ;
#4752 = LINE ( 'NONE', #633, #1441 ) ;
#4753 = CARTESIAN_POINT ( 'NONE',  ( 4.000000000000003553, 0.000000000000000000, 3.500000000000000000 ) ) ;
#4754 = EDGE_LOOP ( 'NONE', ( #4190, #707, #3483, #4268 ) ) ;
#4755 = CARTESIAN_POINT ( 'NONE',  ( 0.000000000000000000, 0.000000000000000000, -32.00000000000000000 ) ) ;
#4756 = ADVANCED_FACE ( 'NONE', ( #550 ), #2076, .T. ) ;
#4757 = CARTESIAN_POINT ( 'NONE',  ( 0.000000000000000000, 0.8865213383406685965, -1.535500000000000753 ) ) ;
#4758 = VERTEX_POINT ( 'NONE', #2403 ) ;
#4759 = AXIS2_PLACEMENT_3D ( 'NONE', #4805, #1001, #4377 ) ;
#4760 = DIRECTION ( 'NONE',  ( 0.000000000000000000, 0.000000000000000000, 1.000000000000000000 ) ) ;
#4761 = APPLICATION_PROTOCOL_DEFINITION ( 'draft international standard', 'automotive_design', 1998, #2667 ) ;
#4762 = EDGE_CURVE ( 'NONE', #1580, #2498, #4393, .T. ) ;
#4763 = SURFACE_SIDE_STYLE ('',( #2790 ) ) ;
#4764 = DIRECTION ( 'NONE',  ( 0.000000000000000000, 0.000000000000000000, 1.000000000000000000 ) ) ;
#4765 = ORIENTED_EDGE ( 'NONE', *, *, #4789, .F. ) ;
#4766 = VERTEX_POINT ( 'NONE', #1717 ) ;
#4767 = EDGE_CURVE ( 'NONE', #1313, #1400, #93, .T. ) ;
#4768 = EDGE_CURVE ( 'NONE', #1912, #537, #3522, .T. ) ;
#4769 = EDGE_CURVE ( 'NONE', #2491, #313, #4678, .T. ) ;
#4770 = CARTESIAN_POINT ( 'NONE',  ( 0.000000000000000000, -25.00000000000000000, -32.00000000000000000 ) ) ;
#4771 = DIRECTION ( 'NONE',  ( -0.000000000000000000, -0.000000000000000000, -1.000000000000000000 ) ) ;
#4772 = CARTESIAN_POINT ( 'NONE',  ( 0.000000000000000000, -2.357898499370432610, 3.252606517456513302E-15 ) ) ;
#4773 = EDGE_LOOP ( 'NONE', ( #1472, #1864 ) ) ;
#4774 = ORIENTED_EDGE ( 'NONE', *, *, #3059, .F. ) ;
#4775 = CARTESIAN_POINT ( 'NONE',  ( 5.200000000000002842, 3.061616997868384127E-16, -2.500000000000000888 ) ) ;
#4776 = CARTESIAN_POINT ( 'NONE',  ( 2.000000000000000000, -1.773042676681340968, 2.059984127722458425E-15 ) ) ;
#4777 = ORIENTED_EDGE ( 'NONE', *, *, #146, .F. ) ;
#4778 = CARTESIAN_POINT ( 'NONE',  ( 2.500000000000000000, 2.500728763858895382E-16, -2.041999999999999815 ) ) ;
#4779 = DIRECTION ( 'NONE',  ( 1.000000000000000000, -0.000000000000000000, -0.000000000000000000 ) ) ;
#4780 = ORIENTED_EDGE ( 'NONE', *, *, #4785, .T. ) ;
#4781 = CARTESIAN_POINT ( 'NONE',  ( 15.00000000000000000, 20.00000000000000355, -32.00000000000000000 ) ) ;
#4782 = APPLICATION_PROTOCOL_DEFINITION ( 'draft international standard', 'automotive_design', 1998, #4288 ) ;
#4783 = DIRECTION ( 'NONE',  ( 1.000000000000000000, -0.000000000000000000, 0.000000000000000000 ) ) ;
#4784 = ORIENTED_EDGE ( 'NONE', *, *, #1703, .T. ) ;
#4785 = EDGE_CURVE ( 'NONE', #1343, #148, #631, .T. ) ;
#4786 = DIRECTION ( 'NONE',  ( 0.000000000000000000, 0.000000000000000000, -1.000000000000000000 ) ) ;
#4787 = PLANE ( 'NONE',  #4008 ) ;
#4788 = DIRECTION ( 'NONE',  ( 0.3199999999999996736, 0.9474175425861610655, 0.000000000000000000 ) ) ;
#4789 = EDGE_CURVE ( 'NONE', #1819, #4296, #4299, .T. ) ;
#4790 = ADVANCED_FACE ( 'NONE', ( #1253 ), #1033, .F. ) ;
#4791 = ORIENTED_EDGE ( 'NONE', *, *, #4921, .T. ) ;
#4792 = ORIENTED_EDGE ( 'NONE', *, *, #3267, .F. ) ;
#4793 = SHAPE_REPRESENTATION_RELATIONSHIP ( 'NONE' , 'NONE' ,  #4748, #996 ) ;
#4794 = CARTESIAN_POINT ( 'NONE',  ( 2.000000000000000000, 0.000000000000000000, 0.000000000000000000 ) ) ;
#4795 = DIRECTION ( 'NONE',  ( 0.000000000000000000, -1.224646799147353454E-16, 1.000000000000000000 ) ) ;
#4796 = CARTESIAN_POINT ( 'NONE',  ( -9.000000000000001776, 3.903127820947817540E-15, -20.00000000000000000 ) ) ;
#4797 = EDGE_CURVE ( 'NONE', #1443, #1262, #2318, .T. ) ;
#4798 = ORIENTED_EDGE ( 'NONE', *, *, #8, .F. ) ;
#4799 = AXIS2_PLACEMENT_3D ( 'NONE', #2911, #4878, #351 ) ;
#4800 = DIRECTION ( 'NONE',  ( -1.000000000000000000, 0.000000000000000000, 0.000000000000000000 ) ) ;
#4801 = CARTESIAN_POINT ( 'NONE',  ( 22.30741055306794962, -11.28818263778243924, -32.00000000000004263 ) ) ;
#4802 = VERTEX_POINT ( 'NONE', #2806 ) ;
#4803 = VECTOR ( 'NONE', #3501, 1000.000000000000000 ) ;
#4804 = CARTESIAN_POINT ( 'NONE',  ( 15.00000000000000000, 16.00000000000000000, -20.00000000000000000 ) ) ;
#4805 = CARTESIAN_POINT ( 'NONE',  ( 0.000000000000000000, 0.000000000000000000, -12.00000000000000000 ) ) ;
#4806 = DIRECTION ( 'NONE',  ( 1.000000000000000000, 0.000000000000000000, 0.000000000000000000 ) ) ;
#4807 = PLANE ( 'NONE',  #4176 ) ;
#4808 = CONICAL_SURFACE ( 'NONE', #3288, 2.099999999999997868, 1.029744258676654090 ) ;
#4809 = EDGE_LOOP ( 'NONE', ( #813, #2958 ) ) ;
#4810 = VECTOR ( 'NONE', #3783, 1000.000000000000000 ) ;
#4811 = AXIS2_PLACEMENT_3D ( 'NONE', #1034, #3734, #2237 ) ;
#4812 = ADVANCED_FACE ( 'NONE', ( #3575 ), #3206, .T. ) ;
#4813 = LINE ( 'NONE', #2821, #4654 ) ;
#4814 = DIRECTION ( 'NONE',  ( -1.000000000000000000, 0.000000000000000000, 0.000000000000000000 ) ) ;
#4815 = DIRECTION ( 'NONE',  ( 0.000000000000000000, 0.000000000000000000, 1.000000000000000000 ) ) ;
#4816 = AXIS2_PLACEMENT_3D ( 'NONE', #205, #224, #2815 ) ;
#4817 = AXIS2_PLACEMENT_3D ( 'NONE', #2257, #4475, #4127 ) ;
#4818 = ORIENTED_EDGE ( 'NONE', *, *, #3528, .F. ) ;
#4819 = PRODUCT_DEFINITION_SHAPE ( 'NONE', 'NONE',  #2684 ) ;
#4820 = ORIENTED_EDGE ( 'NONE', *, *, #541, .F. ) ;
#4821 = AXIS2_PLACEMENT_3D ( 'NONE', #2614, #4788, #4153 ) ;
#4822 = CARTESIAN_POINT ( 'NONE',  ( 0.000000000000000000, 0.000000000000000000, -32.00000000000000000 ) ) ;
#4823 = VECTOR ( 'NONE', #502, 1000.000000000000000 ) ;
#4824 = DIRECTION ( 'NONE',  ( -1.000000000000000000, -0.000000000000000000, -0.000000000000000000 ) ) ;
#4825 = EDGE_CURVE ( 'NONE', #2929, #4351, #3669, .T. ) ;
#4826 = DIRECTION ( 'NONE',  ( 0.000000000000000000, 0.000000000000000000, -1.000000000000000000 ) ) ;
#4827 = EDGE_LOOP ( 'NONE', ( #2448, #1833, #3887, #1719 ) ) ;
#4828 = VECTOR ( 'NONE', #3896, 1000.000000000000000 ) ;
#4829 = DIRECTION ( 'NONE',  ( 1.000000000000000000, -0.000000000000000000, -0.000000000000000000 ) ) ;
#4830 = EDGE_CURVE ( 'NONE', #3603, #4310, #3185, .T. ) ;
#4831 = DIRECTION ( 'NONE',  ( 0.000000000000000000, 0.000000000000000000, -1.000000000000000000 ) ) ;
#4832 = EDGE_CURVE ( 'NONE', #3363, #212, #2726, .T. ) ;
#4833 = ORIENTED_EDGE ( 'NONE', *, *, #4698, .T. ) ;
#4834 = DIRECTION ( 'NONE',  ( 1.000000000000000000, 0.000000000000000000, 0.000000000000000000 ) ) ;
#4835 = FACE_OUTER_BOUND ( 'NONE', #933, .T. ) ;
#4836 = CARTESIAN_POINT ( 'NONE',  ( 22.76747806470417856, -10.32821797429374833, -27.99768719324571364 ) ) ;
#4837 = VECTOR ( 'NONE', #1164, 1000.000000000000000 ) ;
#4838 = VERTEX_POINT ( 'NONE', #4490 ) ;
#4839 = CARTESIAN_POINT ( 'NONE',  ( 22.47483654244695472, 10.94974330264383511, -22.75458106415069182 ) ) ;
#4840 = DIRECTION ( 'NONE',  ( 0.000000000000000000, 0.000000000000000000, -1.000000000000000000 ) ) ;
#4841 = CARTESIAN_POINT ( 'NONE',  ( 0.000000000000000000, 0.000000000000000000, -32.00000000000000000 ) ) ;
#4842 = VERTEX_POINT ( 'NONE', #689 ) ;
#4843 = ORIENTED_EDGE ( 'NONE', *, *, #2651, .F. ) ;
#4844 = FILL_AREA_STYLE_COLOUR ( '', #4862 ) ;
#4845 = CARTESIAN_POINT ( 'NONE',  ( 4.196500603111122875E-14, 12.50000000000000178, -12.00000000000000000 ) ) ;
#4846 = DIRECTION ( 'NONE',  ( 0.000000000000000000, 0.000000000000000000, -1.000000000000000000 ) ) ;
#4847 = ORIENTED_EDGE ( 'NONE', *, *, #3258, .F. ) ;
#4848 = CARTESIAN_POINT ( 'NONE',  ( 0.000000000000000000, 0.000000000000000000, -20.00000000000000000 ) ) ;
#4849 = VERTEX_POINT ( 'NONE', #4873 ) ;
#4850 = VERTEX_POINT ( 'NONE', #315 ) ;
#4851 = DIRECTION ( 'NONE',  ( -0.000000000000000000, -0.000000000000000000, 1.000000000000000000 ) ) ;
#4852 = DIRECTION ( 'NONE',  ( 0.000000000000000000, 0.000000000000000000, -1.000000000000000000 ) ) ;
#4853 = DIRECTION ( 'NONE',  ( -1.000000000000000000, -0.000000000000000000, -0.000000000000000000 ) ) ;
#4854 = ORIENTED_EDGE ( 'NONE', *, *, #4855, .F. ) ;
#4855 = EDGE_CURVE ( 'NONE', #1390, #4372, #2485, .T. ) ;
#4856 = ADVANCED_FACE ( 'NONE', ( #1433 ), #1017, .F. ) ;
#4857 = CARTESIAN_POINT ( 'NONE',  ( 2.444036937190193033E-14, 6.999999999999999112, -32.00000000000000000 ) ) ;
#4858 = DIRECTION ( 'NONE',  ( -0.000000000000000000, -0.000000000000000000, -1.000000000000000000 ) ) ;
#4859 = VERTEX_POINT ( 'NONE', #2927 ) ;
#4860 = EDGE_CURVE ( 'NONE', #2945, #4443, #1834, .T. ) ;
#4861 = CARTESIAN_POINT ( 'NONE',  ( 3.678949249685231848, 0.000000000000000000, 0.000000000000000000 ) ) ;
#4862 = COLOUR_RGB ( '', 0.31764706, 0.68627451, 0.89019608) ;
#4863 = CARTESIAN_POINT ( 'NONE',  ( 8.500000000000001776, -9.407539813567788568E-16, 4.000000000000000000 ) ) ;
#4864 = DIRECTION ( 'NONE',  ( -0.000000000000000000, 0.000000000000000000, 1.000000000000000000 ) ) ;
#4865 = EDGE_LOOP ( 'NONE', ( #3499, #4898, #1535, #3118 ) ) ;
#4866 = VERTEX_POINT ( 'NONE', #4440 ) ;
#4867 =( NAMED_UNIT ( * ) PLANE_ANGLE_UNIT ( ) SI_UNIT ( $, .RADIAN. ) );
#4868 = DIRECTION ( 'NONE',  ( 0.000000000000000000, 1.000000000000000000, -1.224646799147353207E-16 ) ) ;
#4869 = LINE ( 'NONE', #2238, #332 ) ;
#4870 = DIRECTION ( 'NONE',  ( 0.000000000000000000, 0.000000000000000000, -1.000000000000000000 ) ) ;
#4871 = ORIENTED_EDGE ( 'NONE', *, *, #2643, .F. ) ;
#4872 = DIRECTION ( 'NONE',  ( -1.000000000000000000, 0.000000000000000000, 0.000000000000000000 ) ) ;
#4873 = CARTESIAN_POINT ( 'NONE',  ( 15.00000000000000178, -16.00000000000000000, -23.35000000000001563 ) ) ;
#4874 = LINE ( 'NONE', #1488, #1759 ) ;
#4875 = ADVANCED_FACE ( 'NONE', ( #1464 ), #2546, .T. ) ;
#4876 = VECTOR ( 'NONE', #3376, 1000.000000000000000 ) ;
#4877 = ORIENTED_EDGE ( 'NONE', *, *, #2066, .T. ) ;
#4878 = DIRECTION ( 'NONE',  ( 0.3200000000000010614, -0.9474175425861606215, 0.000000000000000000 ) ) ;
#4879 = AXIS2_PLACEMENT_3D ( 'NONE', #3369, #668, #294 ) ;
#4880 = CARTESIAN_POINT ( 'NONE',  ( 0.000000000000000000, 0.000000000000000000, 4.000000000000000000 ) ) ;
#4881 = CARTESIAN_POINT ( 'NONE',  ( 2.500000000000000000, 2.357898499370433054, -1.951563910473907981E-15 ) ) ;
#4882 = EDGE_CURVE ( 'NONE', #3640, #1343, #3643, .T. ) ;
#4883 = ORIENTED_EDGE ( 'NONE', *, *, #4547, .F. ) ;
#4884 = AXIS2_PLACEMENT_3D ( 'NONE', #2434, #3109, #94 ) ;
#4885 = FACE_BOUND ( 'NONE', #324, .T. ) ;
#4886 = EDGE_CURVE ( 'NONE', #4359, #2811, #4065, .T. ) ;
#4887 = CIRCLE ( 'NONE', #1045, 6.999999999999999112 ) ;
#4888 = CARTESIAN_POINT ( 'NONE',  ( 2.500000000000000000, 0.000000000000000000, 0.000000000000000000 ) ) ;
#4889 = CARTESIAN_POINT ( 'NONE',  ( 12.49999999999999822, -19.30673457630782863, 4.000000000000000000 ) ) ;
#4890 = ORIENTED_EDGE ( 'NONE', *, *, #1254, .T. ) ;
#4891 = CONICAL_SURFACE ( 'NONE', #3460, 2.099999999999997868, 1.029744258676654090 ) ;
#4892 = VERTEX_POINT ( 'NONE', #2175 ) ;
#4893 = LINE ( 'NONE', #3000, #2979 ) ;
#4894 = DIRECTION ( 'NONE',  ( -0.000000000000000000, -0.000000000000000000, 1.000000000000000000 ) ) ;
#4895 = AXIS2_PLACEMENT_3D ( 'NONE', #1556, #3885, #1236 ) ;
#4896 = DIRECTION ( 'NONE',  ( 1.000000000000000000, -0.000000000000000000, -0.000000000000000000 ) ) ;
#4897 = AXIS2_PLACEMENT_3D ( 'NONE', #4053, #2960, #4500 ) ;
#4898 = ORIENTED_EDGE ( 'NONE', *, *, #489, .T. ) ;
#4899 = CONICAL_SURFACE ( 'NONE', #3693, 25.00000000000000000, 0.7853981633974500554 ) ;
#4900 = CIRCLE ( 'NONE', #2029, 6.999999999999999112 ) ;
#4901 = CARTESIAN_POINT ( 'NONE',  ( 2.444036937190193033E-14, 6.999999999999999112, -32.00000000000000000 ) ) ;
#4902 = DIRECTION ( 'NONE',  ( -0.000000000000000000, -0.000000000000000000, 1.000000000000000000 ) ) ;
#4903 = LINE ( 'NONE', #3371, #1437 ) ;
#4904 =( LENGTH_UNIT ( ) NAMED_UNIT ( * ) SI_UNIT ( .MILLI., .METRE. ) );
#4905 = VECTOR ( 'NONE', #2703, 1000.000000000000000 ) ;
#4906 = EDGE_LOOP ( 'NONE', ( #4366, #1180, #4605, #4291 ) ) ;
#4907 = VECTOR ( 'NONE', #2209, 1000.000000000000000 ) ;
#4908 = CARTESIAN_POINT ( 'NONE',  ( 5.000000000000002665, 3.306546357697854226E-16, 2.700000000000001066 ) ) ;
#4909 = DIRECTION ( 'NONE',  ( 0.000000000000000000, 0.000000000000000000, -1.000000000000000000 ) ) ;
#4910 = ORIENTED_EDGE ( 'NONE', *, *, #2627, .F. ) ;
#4911 = EDGE_CURVE ( 'NONE', #9, #4410, #3723, .T. ) ;
#4912 = EDGE_CURVE ( 'NONE', #4937, #1467, #399, .T. ) ;
#4913 = DIRECTION ( 'NONE',  ( 0.000000000000000000, -1.000000000000000000, 0.000000000000000000 ) ) ;
#4914 = DIRECTION ( 'NONE',  ( 1.000000000000000000, 0.000000000000000000, 0.000000000000000000 ) ) ;
#4915 = CARTESIAN_POINT ( 'NONE',  ( 2.000000000000000000, 1.773042676681340968, -2.276824562219559311E-15 ) ) ;
#4916 = PLANE ( 'NONE',  #1376 ) ;
#4917 = ORIENTED_EDGE ( 'NONE', *, *, #1242, .F. ) ;
#4918 = AXIS2_PLACEMENT_3D ( 'NONE', #203, #1398, #2932 ) ;
#4919 = ADVANCED_FACE ( 'NONE', ( #4043, #2571 ), #2222, .T. ) ;
#4920 = ADVANCED_FACE ( 'NONE', ( #3302 ), #1817, .F. ) ;
#4921 = EDGE_CURVE ( 'NONE', #675, #4685, #3832, .T. ) ;
#4922 = EDGE_LOOP ( 'NONE', ( #273, #1813, #2224, #4126 ) ) ;
#4923 = DIRECTION ( 'NONE',  ( 0.000000000000000000, 0.000000000000000000, 1.000000000000000000 ) ) ;
#4924 = LINE ( 'NONE', #289, #173 ) ;
#4925 = DIRECTION ( 'NONE',  ( 0.000000000000000000, 0.000000000000000000, -1.000000000000000000 ) ) ;
#4926 = DIRECTION ( 'NONE',  ( -1.000000000000000000, 0.000000000000000000, -0.000000000000000000 ) ) ;
#4927 = ORIENTED_EDGE ( 'NONE', *, *, #4797, .T. ) ;
#4928 = EDGE_LOOP ( 'NONE', ( #2149, #2754, #1005, #3111, #1882, #2117, #3908, #542 ) ) ;
#4929 = DIRECTION ( 'NONE',  ( 0.000000000000000000, 0.000000000000000000, -1.000000000000000000 ) ) ;
#4930 = SURFACE_STYLE_FILL_AREA ( #814 ) ;
#4931 = CARTESIAN_POINT ( 'NONE',  ( 24.55500000000002103, 0.000000000000000000, 0.000000000000000000 ) ) ;
#4932 =( LENGTH_UNIT ( ) NAMED_UNIT ( * ) SI_UNIT ( .MILLI., .METRE. ) );
#4933 = ORIENTED_EDGE ( 'NONE', *, *, #2131, .F. ) ;
#4934 = CARTESIAN_POINT ( 'NONE',  ( -9.000000000000003553, -1.999999999999999112, -32.00000000000000000 ) ) ;
#4935 = SURFACE_STYLE_USAGE ( .BOTH. , #3351 ) ;
#4936 = CONTEXT_DEPENDENT_SHAPE_REPRESENTATION ( #2836, #1650 ) ;
#4937 = VERTEX_POINT ( 'NONE', #3664 ) ;
#4938 = PRODUCT_DEFINITION_CONTEXT ( 'detailed design', #4442, 'design' ) ;
#4939 = CARTESIAN_POINT ( 'NONE',  ( 2.444036937190193033E-14, 6.999999999999999112, -20.00000000000000000 ) ) ;
#4940 = CARTESIAN_POINT ( 'NONE',  ( 0.000000000000000000, 0.000000000000000000, 14.30577747056276472 ) ) ;
#4941 = DIRECTION ( 'NONE',  ( -1.000000000000000000, -0.000000000000000000, -0.000000000000000000 ) ) ;
#4942 = CARTESIAN_POINT ( 'NONE',  ( 24.00000000000000000, 1.971681346627238735E-16, -1.610000000000000098 ) ) ;
#4943 = EDGE_CURVE ( 'NONE', #811, #121, #4317, .T. ) ;
#4944 = EDGE_LOOP ( 'NONE', ( #1570, #2770, #2683, #2474 ) ) ;
#4945 = STYLED_ITEM ( 'NONE', ( #1136 ), #1407 ) ;
#4946 = PLANE ( 'NONE',  #361 ) ;
#4947 = DIRECTION ( 'NONE',  ( 0.02118582507427613226, 0.9997755552202316487, 9.765537692533071851E-17 ) ) ;
#4948 = CARTESIAN_POINT ( 'NONE',  ( 15.00000000000000000, 16.00000000000000000, -32.00000000000000000 ) ) ;
#4949 = PLANE ( 'NONE',  #2251 ) ;
#4950 = FACE_OUTER_BOUND ( 'NONE', #1736, .T. ) ;
#4951 = ORIENTED_EDGE ( 'NONE', *, *, #272, .F. ) ;
#4952 = DIRECTION ( 'NONE',  ( 0.000000000000000000, 0.000000000000000000, 1.000000000000000000 ) ) ;
#4953 = DIRECTION ( 'NONE',  ( 0.000000000000000000, 0.000000000000000000, -1.000000000000000000 ) ) ;
#4954 = FACE_OUTER_BOUND ( 'NONE', #736, .T. ) ;
#4955 = EDGE_CURVE ( 'NONE', #2953, #881, #243, .T. ) ;
#4956 = ORIENTED_EDGE ( 'NONE', *, *, #3748, .F. ) ;
#4957 = DIRECTION ( 'NONE',  ( -1.000000000000000000, -0.000000000000000000, -0.000000000000000000 ) ) ;
#4958 = LINE ( 'NONE', #2629, #924 ) ;
#4959 = VECTOR ( 'NONE', #1122, 1000.000000000000000 ) ;
#4960 = EDGE_LOOP ( 'NONE', ( #912, #4507, #3962, #4167, #2799, #4597 ) ) ;
#4961 = ORIENTED_EDGE ( 'NONE', *, *, #1945, .T. ) ;
#4962 = AXIS2_PLACEMENT_3D ( 'NONE', #277, #1836, #4800 ) ;
#4963 = CARTESIAN_POINT ( 'NONE',  ( 0.000000000000000000, 0.000000000000000000, 0.000000000000000000 ) ) ;
#4964 = NEXT_ASSEMBLY_USAGE_OCCURRENCE ( 'NAUO1', ' ', ' ', #596, #4361, $ ) ;
#4965 = NEXT_ASSEMBLY_USAGE_OCCURRENCE ( 'NAUO2', ' ', ' ', #596, #1181, $ ) ;
#4966 = NEXT_ASSEMBLY_USAGE_OCCURRENCE ( 'NAUO3', ' ', ' ', #596, #2072, $ ) ;
#4967 = NEXT_ASSEMBLY_USAGE_OCCURRENCE ( 'NAUO4', ' ', ' ', #596, #2896, $ ) ;
#4968 = NEXT_ASSEMBLY_USAGE_OCCURRENCE ( 'NAUO5', ' ', ' ', #596, #2072, $ ) ;
#4969 = NEXT_ASSEMBLY_USAGE_OCCURRENCE ( 'NAUO6', ' ', ' ', #596, #2307, $ ) ;
#4970 = NEXT_ASSEMBLY_USAGE_OCCURRENCE ( 'NAUO7', ' ', ' ', #596, #2307, $ ) ;
#4971 = NEXT_ASSEMBLY_USAGE_OCCURRENCE ( 'NAUO8', ' ', ' ', #596, #2684, $ ) ;
#4972 = NEXT_ASSEMBLY_USAGE_OCCURRENCE ( 'NAUO9', ' ', ' ', #596, #2684, $ ) ;
ENDSEC;
END-ISO-10303-21;
